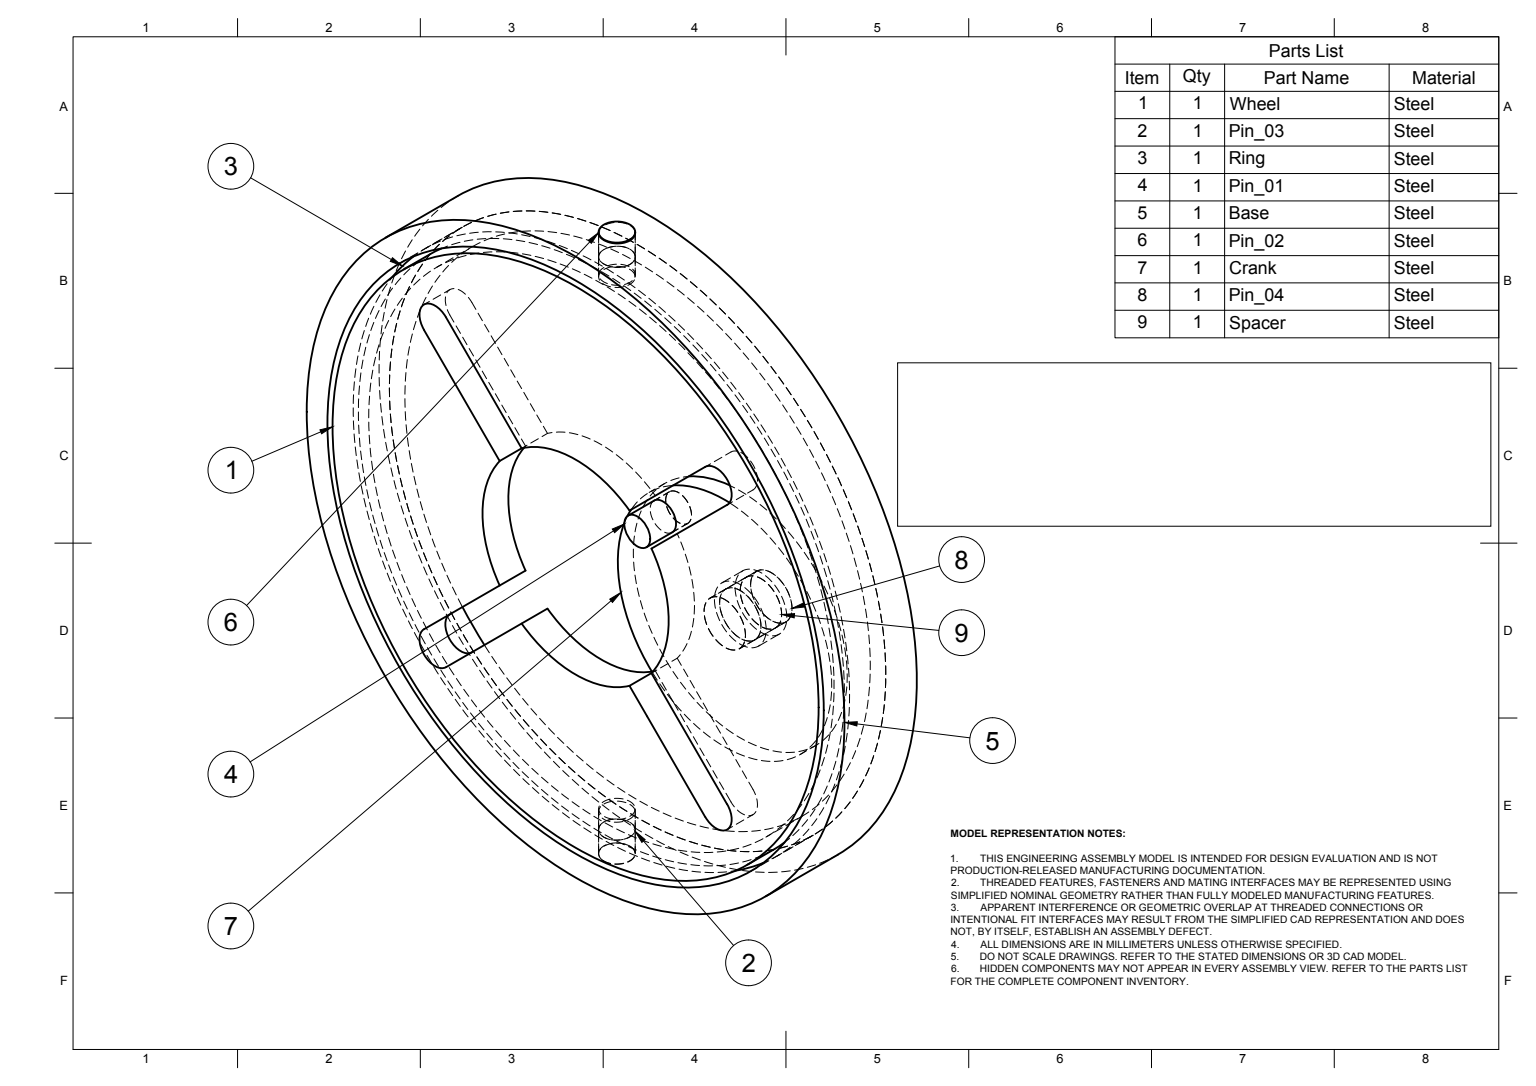
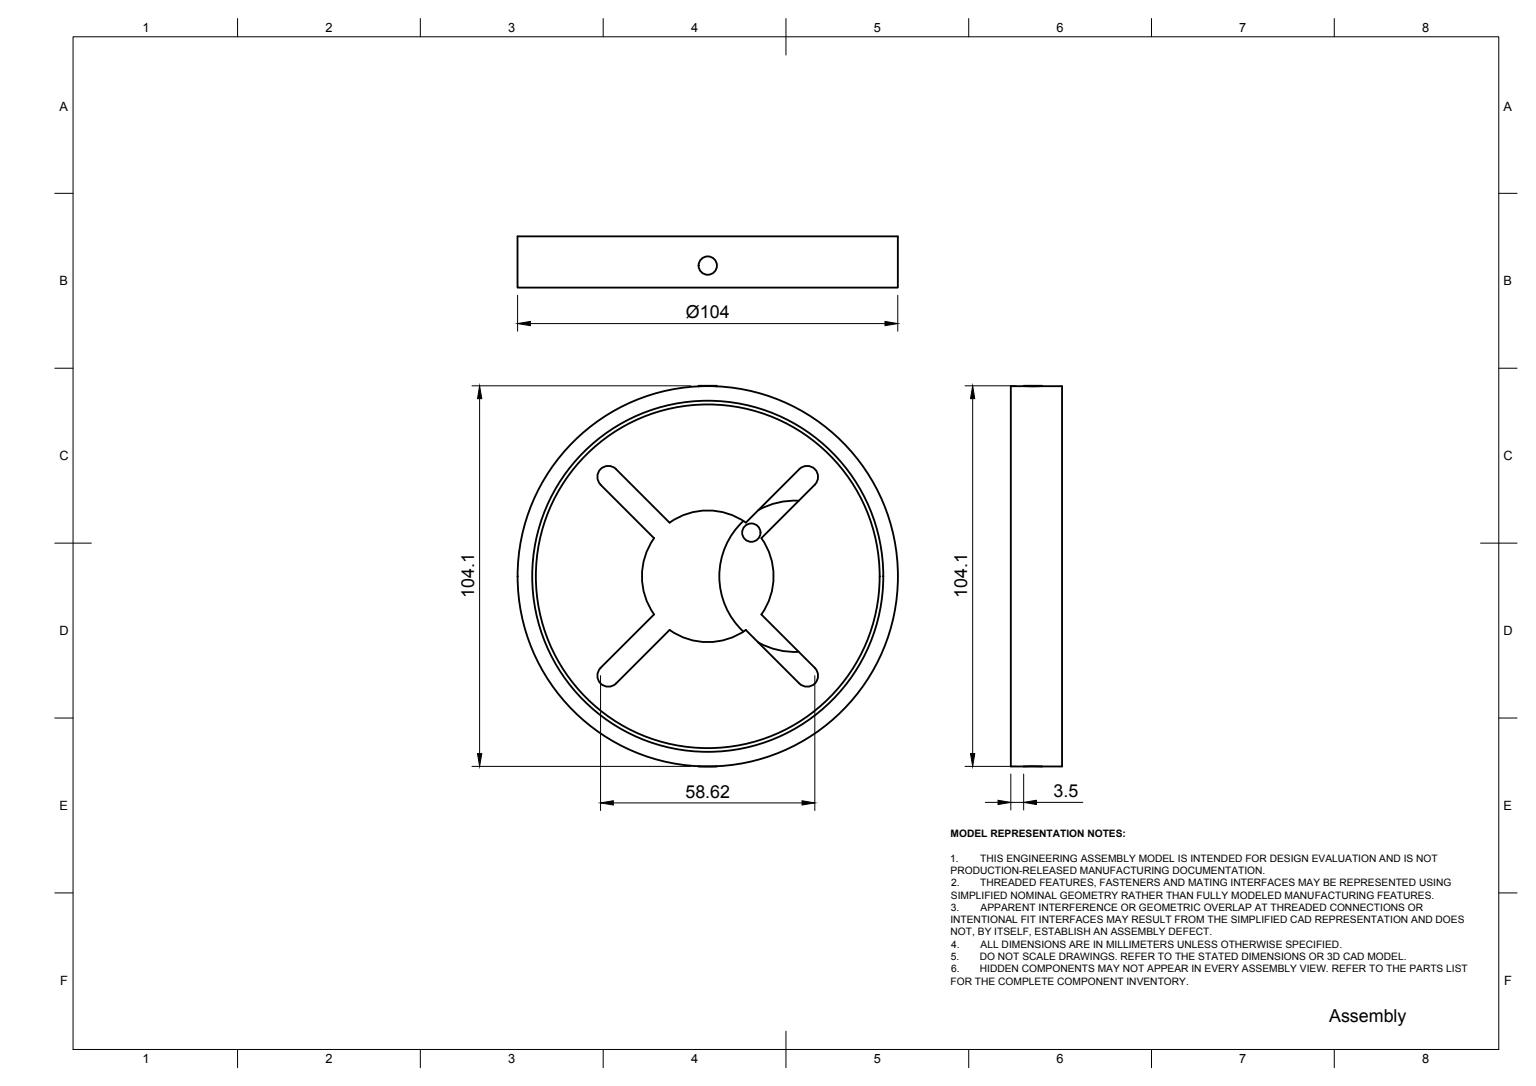
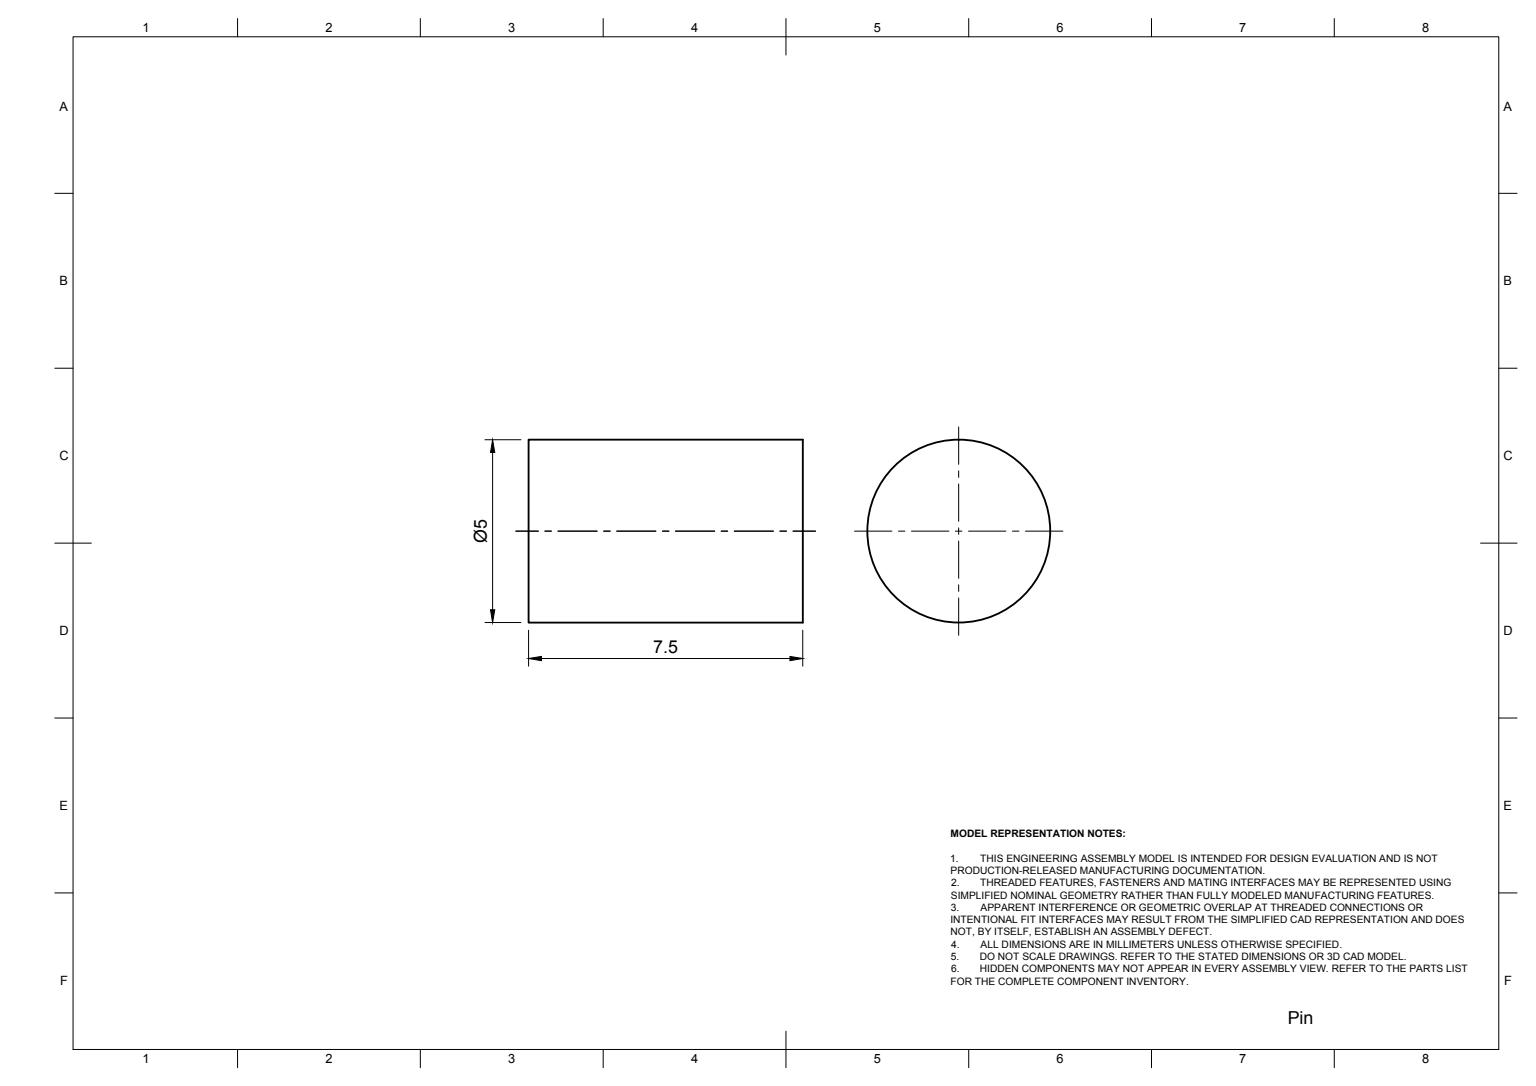
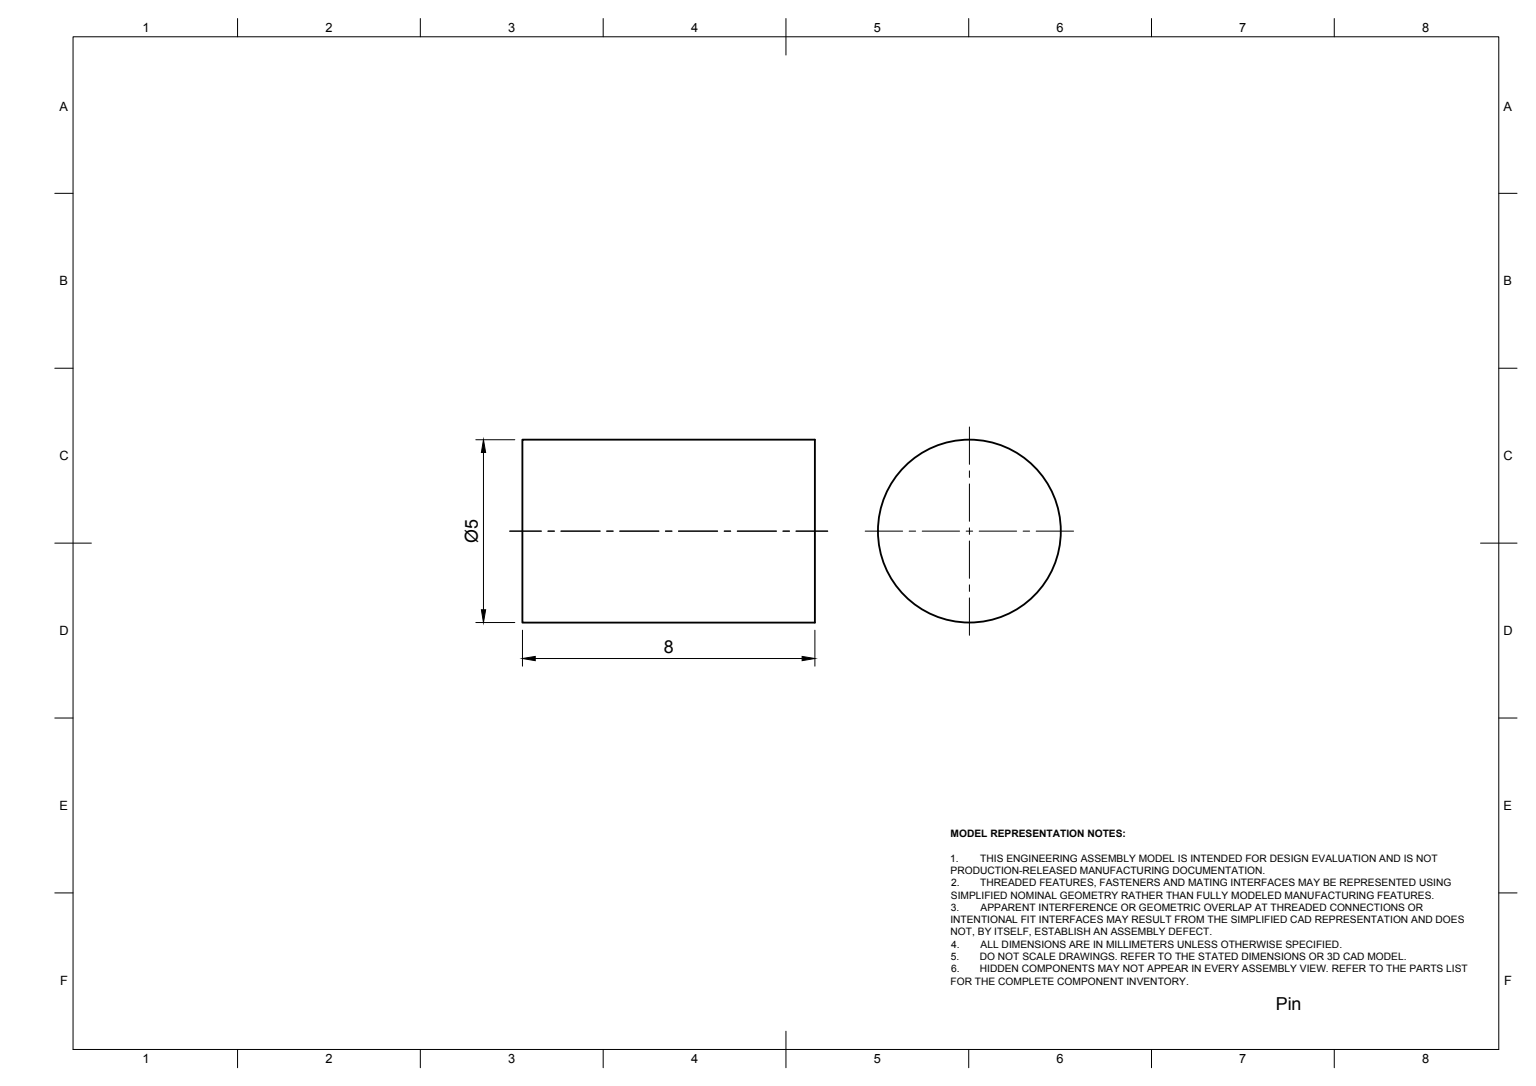
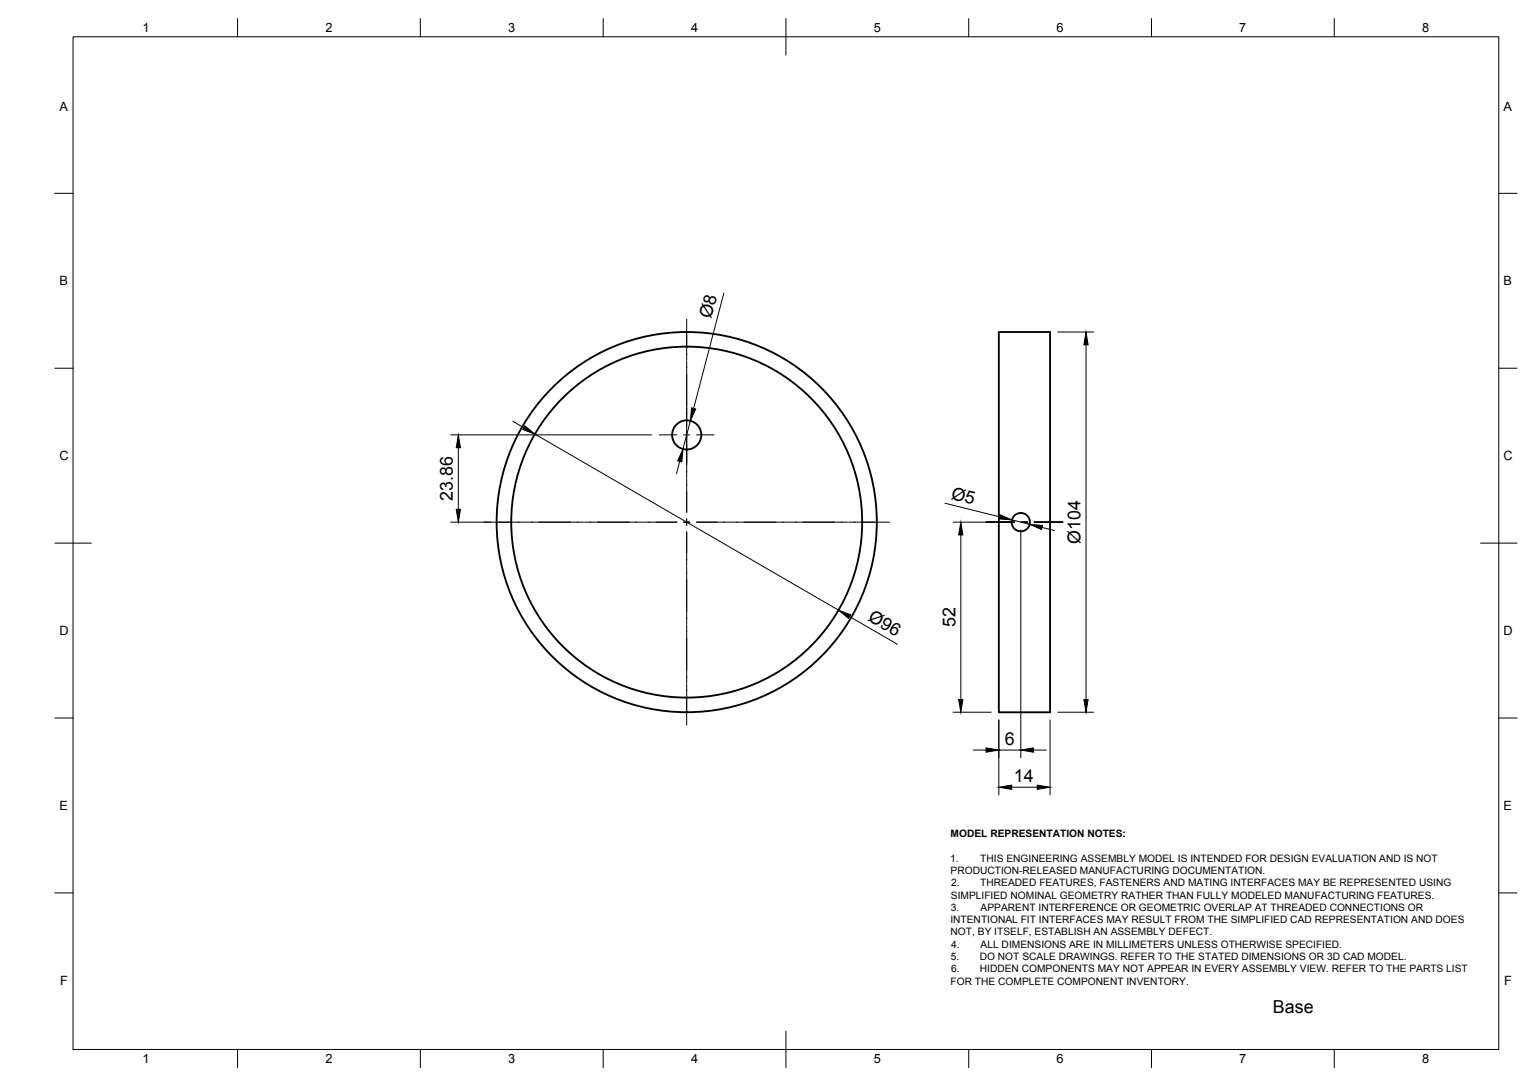
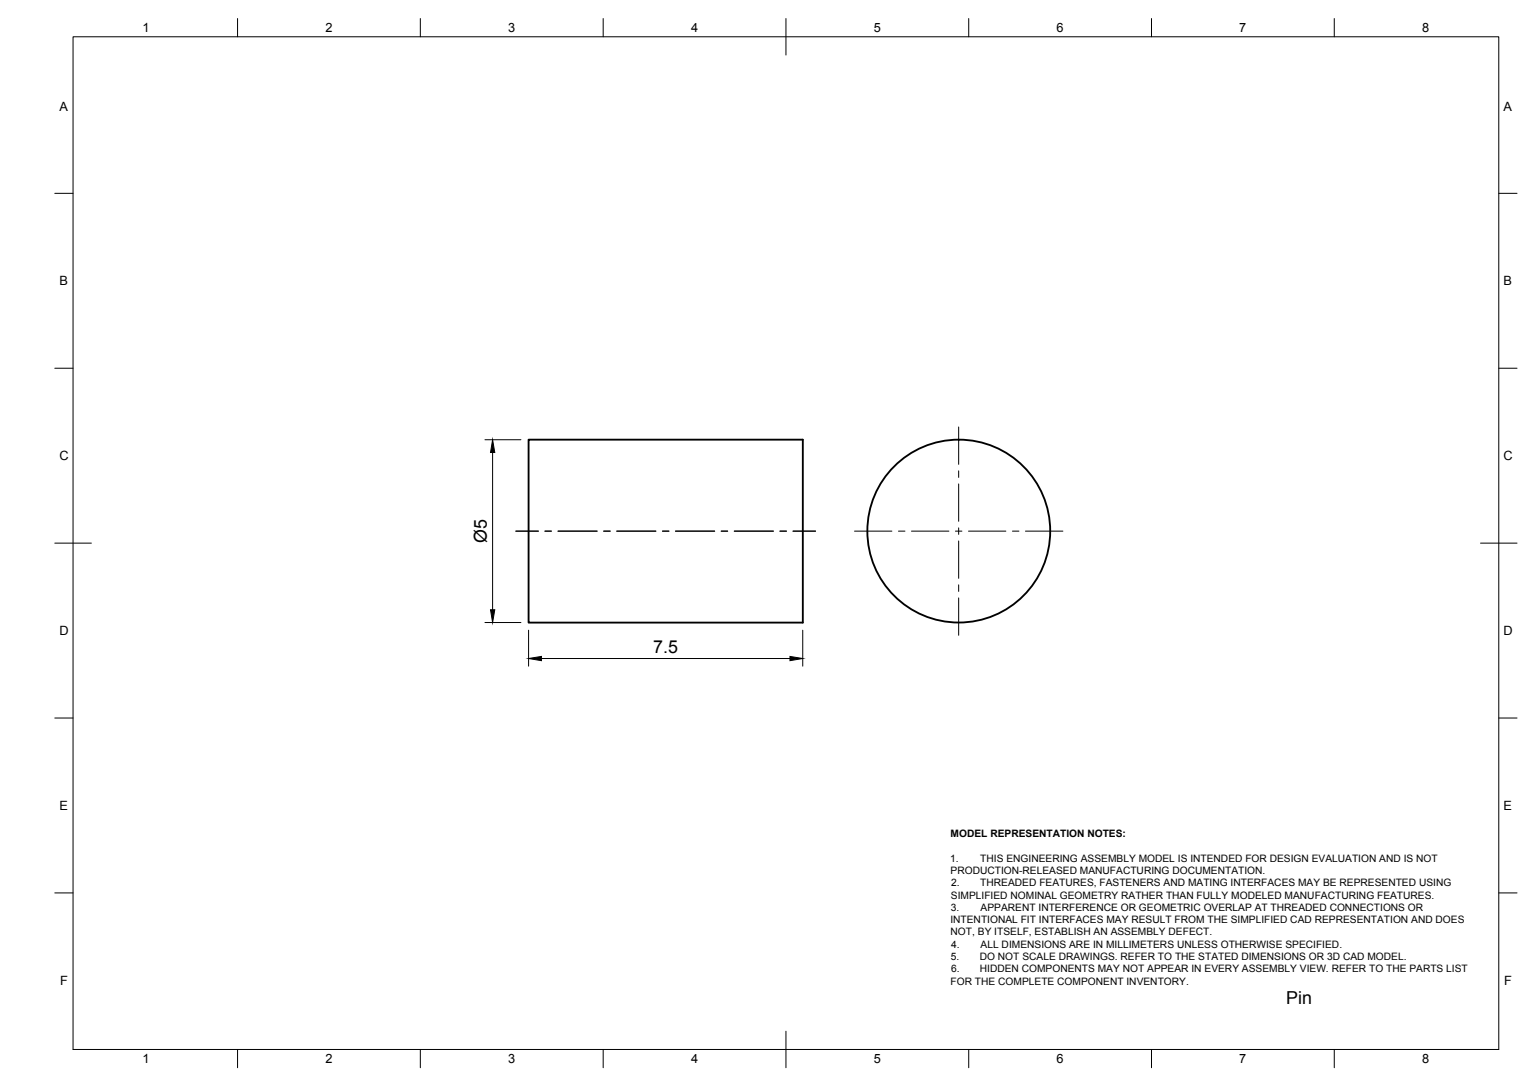
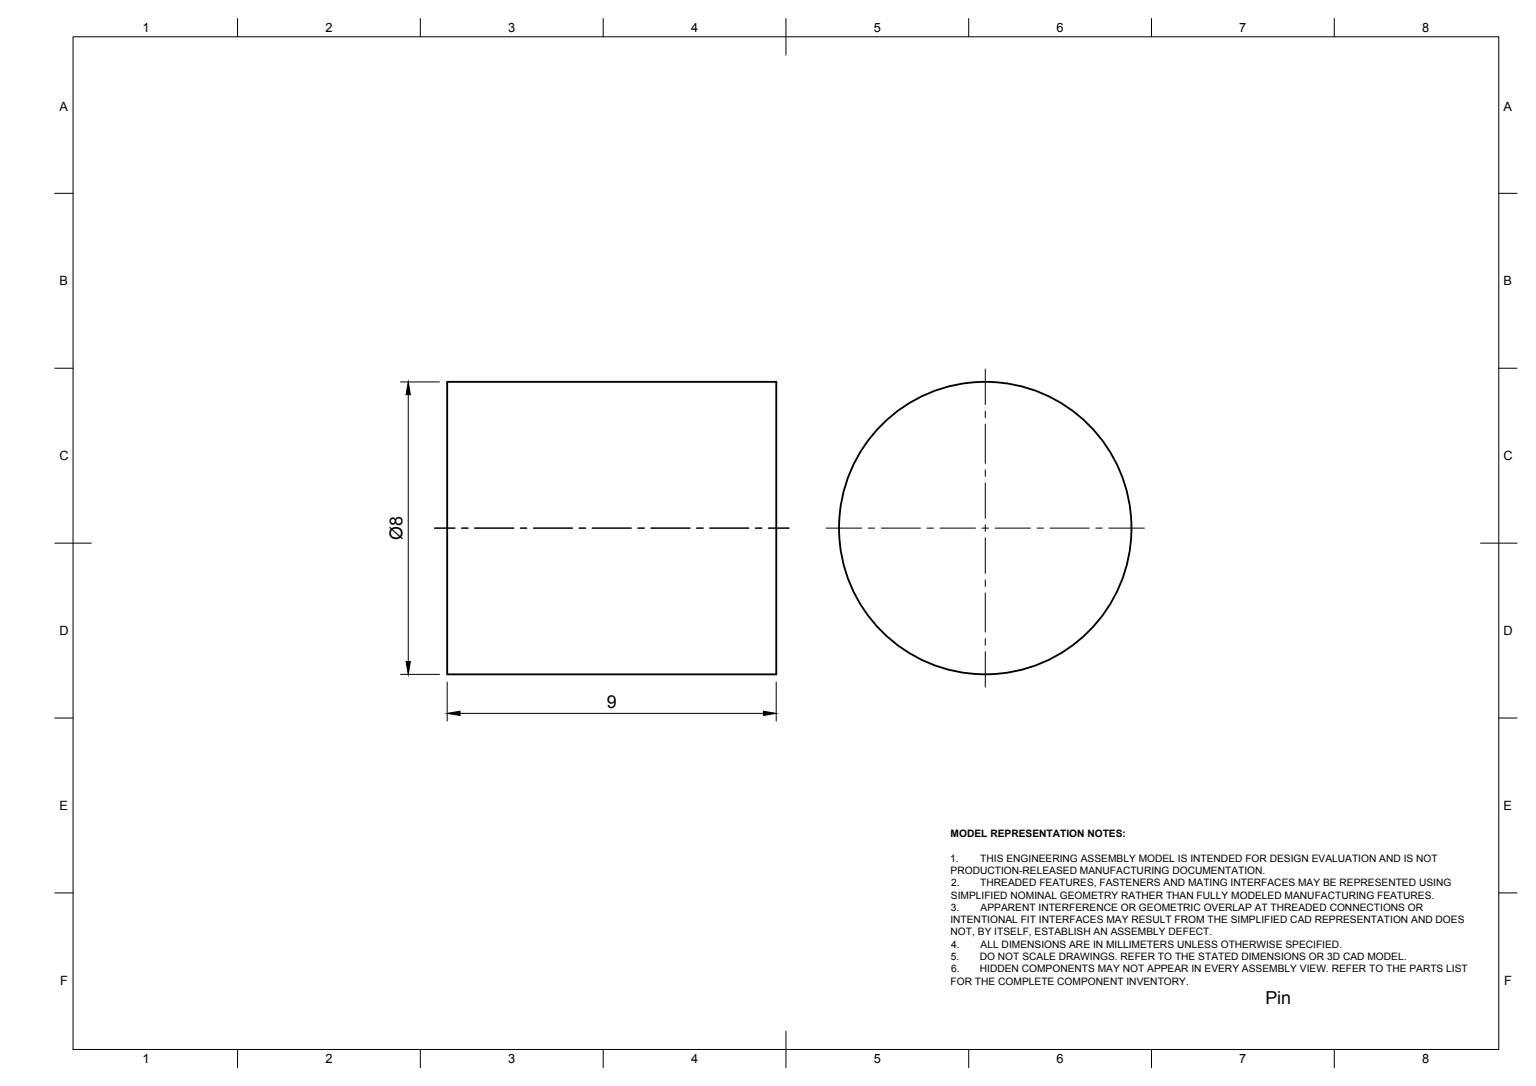
ISO-10303-21;
HEADER;
/* Generated by software containing ST-Developer
 * from STEP Tools, Inc. (www.steptools.com) 
 */

FILE_DESCRIPTION(
/* description */ (''),
/* implementation_level */ '2;1');

FILE_NAME(
/* name */ 'BR-053',
/* time_stamp */ '2026-10-04T12:17:52-07:00',
/* author */ (''),
/* organization */ (''),
/* preprocessor_version */ 'ST-DEVELOPER v20.2',
/* originating_system */ 'Autodesk Translation Framework v15.15.0.0',
/* authorisation */ '');

FILE_SCHEMA (('AUTOMOTIVE_DESIGN { 1 0 10303 214 3 1 1 }'));
ENDSEC;

DATA;
#10=MECHANICAL_DESIGN_GEOMETRIC_PRESENTATION_REPRESENTATION('',(#63,#64,
#65,#66,#67,#68,#69,#70),#1602);
#11=ITEM_DEFINED_TRANSFORMATION($,$,#872,#967);
#12=ITEM_DEFINED_TRANSFORMATION($,$,#911,#968);
#13=ITEM_DEFINED_TRANSFORMATION($,$,#917,#969);
#14=ITEM_DEFINED_TRANSFORMATION($,$,#928,#970);
#15=ITEM_DEFINED_TRANSFORMATION($,$,#934,#971);
#16=ITEM_DEFINED_TRANSFORMATION($,$,#940,#972);
#17=ITEM_DEFINED_TRANSFORMATION($,$,#952,#973);
#18=ITEM_DEFINED_TRANSFORMATION($,$,#958,#974);
#19=(
REPRESENTATION_RELATIONSHIP($,$,#1634,#1633)
REPRESENTATION_RELATIONSHIP_WITH_TRANSFORMATION(#11)
SHAPE_REPRESENTATION_RELATIONSHIP()
);
#20=(
REPRESENTATION_RELATIONSHIP($,$,#1635,#1633)
REPRESENTATION_RELATIONSHIP_WITH_TRANSFORMATION(#12)
SHAPE_REPRESENTATION_RELATIONSHIP()
);
#21=(
REPRESENTATION_RELATIONSHIP($,$,#1636,#1633)
REPRESENTATION_RELATIONSHIP_WITH_TRANSFORMATION(#13)
SHAPE_REPRESENTATION_RELATIONSHIP()
);
#22=(
REPRESENTATION_RELATIONSHIP($,$,#1637,#1633)
REPRESENTATION_RELATIONSHIP_WITH_TRANSFORMATION(#14)
SHAPE_REPRESENTATION_RELATIONSHIP()
);
#23=(
REPRESENTATION_RELATIONSHIP($,$,#1638,#1633)
REPRESENTATION_RELATIONSHIP_WITH_TRANSFORMATION(#15)
SHAPE_REPRESENTATION_RELATIONSHIP()
);
#24=(
REPRESENTATION_RELATIONSHIP($,$,#1639,#1633)
REPRESENTATION_RELATIONSHIP_WITH_TRANSFORMATION(#16)
SHAPE_REPRESENTATION_RELATIONSHIP()
);
#25=(
REPRESENTATION_RELATIONSHIP($,$,#1640,#1633)
REPRESENTATION_RELATIONSHIP_WITH_TRANSFORMATION(#17)
SHAPE_REPRESENTATION_RELATIONSHIP()
);
#26=(
REPRESENTATION_RELATIONSHIP($,$,#1641,#1633)
REPRESENTATION_RELATIONSHIP_WITH_TRANSFORMATION(#18)
SHAPE_REPRESENTATION_RELATIONSHIP()
);
#27=CONTEXT_DEPENDENT_SHAPE_REPRESENTATION(#19,#1625);
#28=CONTEXT_DEPENDENT_SHAPE_REPRESENTATION(#20,#1626);
#29=CONTEXT_DEPENDENT_SHAPE_REPRESENTATION(#21,#1627);
#30=CONTEXT_DEPENDENT_SHAPE_REPRESENTATION(#22,#1628);
#31=CONTEXT_DEPENDENT_SHAPE_REPRESENTATION(#23,#1629);
#32=CONTEXT_DEPENDENT_SHAPE_REPRESENTATION(#24,#1630);
#33=CONTEXT_DEPENDENT_SHAPE_REPRESENTATION(#25,#1631);
#34=CONTEXT_DEPENDENT_SHAPE_REPRESENTATION(#26,#1632);
#35=NEXT_ASSEMBLY_USAGE_OCCURRENCE('Wheel:1','Wheel:1','Wheel:1',#1643,
#1644,'Wheel:1');
#36=NEXT_ASSEMBLY_USAGE_OCCURRENCE('Pin_03:1','Pin_03:1','Pin_03:1',#1643,
#1645,'Pin_03:1');
#37=NEXT_ASSEMBLY_USAGE_OCCURRENCE('Ring:1','Ring:1','Ring:1',#1643,#1646,
'Ring:1');
#38=NEXT_ASSEMBLY_USAGE_OCCURRENCE('Pin_01:1','Pin_01:1','Pin_01:1',#1643,
#1647,'Pin_01:1');
#39=NEXT_ASSEMBLY_USAGE_OCCURRENCE('Pin_02:1','Pin_02:1','Pin_02:1',#1643,
#1648,'Pin_02:1');
#40=NEXT_ASSEMBLY_USAGE_OCCURRENCE('Crank:1','Crank:1','Crank:1',#1643,
#1649,'Crank:1');
#41=NEXT_ASSEMBLY_USAGE_OCCURRENCE('Pin_04:1','Pin_04:1','Pin_04:1',#1643,
#1650,'Pin_04:1');
#42=NEXT_ASSEMBLY_USAGE_OCCURRENCE('Spacer:1','Spacer:1','Spacer:1',#1643,
#1651,'Spacer:1');
#43=B_SPLINE_CURVE_WITH_KNOTS('',3,(#1356,#1357,#1358,#1359,#1360,#1361,
#1362,#1363,#1364,#1365,#1366,#1367,#1368,#1369,#1370,#1371,#1372,#1373,
#1374,#1375,#1376,#1377,#1378,#1379,#1380,#1381,#1382,#1383,#1384,#1385,
#1386,#1387,#1388,#1389),.UNSPECIFIED.,.T.,.F.,(4,2,2,2,2,2,2,2,2,2,2,2,
2,2,2,2,4),(0.,0.0941899649900925,0.188379929980185,0.282569871539204,0.376759813098223,
0.470949754657242,0.565139696216261,0.659329661206353,0.753519626196446,
0.847709591186538,0.941899556176631,1.03608949773565,1.13027943929467,1.22446938085369,
1.31865932241271,1.4128492874028,1.50703925239289),.UNSPECIFIED.);
#44=B_SPLINE_CURVE_WITH_KNOTS('',3,(#1392,#1393,#1394,#1395,#1396,#1397,
#1398,#1399,#1400,#1401,#1402,#1403,#1404,#1405,#1406,#1407,#1408,#1409,
#1410,#1411,#1412,#1413,#1414,#1415,#1416,#1417,#1418,#1419,#1420,#1421,
#1422,#1423,#1424,#1425),.UNSPECIFIED.,.T.,.F.,(4,2,2,2,2,2,2,2,2,2,2,2,
2,2,2,2,4),(-1.50707960704781,-1.41288711643541,-1.318694625823,-1.22450216555443,
-1.13030970528586,-1.03611724501729,-0.941924784748718,-0.847732294136312,
-0.753539803523906,-0.6593473129115,-0.565154822299094,-0.470962362030524,
-0.376769901761953,-0.282577441493383,-0.188384981224812,-0.094192490612406,
0.),.UNSPECIFIED.);
#45=B_SPLINE_CURVE_WITH_KNOTS('',3,(#1428,#1429,#1430,#1431,#1432,#1433,
#1434,#1435,#1436,#1437,#1438,#1439,#1440,#1441,#1442,#1443,#1444,#1445,
#1446,#1447,#1448,#1449,#1450,#1451,#1452,#1453,#1454,#1455,#1456,#1457,
#1458,#1459,#1460,#1461),.UNSPECIFIED.,.T.,.F.,(4,2,2,2,2,2,2,2,2,2,2,2,
2,2,2,2,4),(-1.50707960704781,-1.41288711643541,-1.318694625823,-1.22450216555443,
-1.13030970528586,-1.03611724501729,-0.941924784748719,-0.847732294136313,
-0.753539803523906,-0.6593473129115,-0.565154822299094,-0.470962362030524,
-0.376769901761953,-0.282577441493383,-0.188384981224812,-0.0941924906124062,
0.),.UNSPECIFIED.);
#46=B_SPLINE_CURVE_WITH_KNOTS('',3,(#1464,#1465,#1466,#1467,#1468,#1469,
#1470,#1471,#1472,#1473,#1474,#1475,#1476,#1477,#1478,#1479,#1480,#1481,
#1482,#1483,#1484,#1485,#1486,#1487,#1488,#1489,#1490,#1491,#1492,#1493,
#1494,#1495,#1496,#1497),.UNSPECIFIED.,.T.,.F.,(4,2,2,2,2,2,2,2,2,2,2,2,
2,2,2,2,4),(0.,0.0941899649900927,0.188379929980185,0.282569871539204,0.376759813098223,
0.470949754657242,0.565139696216261,0.659329661206353,0.753519626196446,
0.847709591186538,0.941899556176631,1.03608949773565,1.13027943929467,1.22446938085369,
1.31865932241271,1.4128492874028,1.50703925239289),.UNSPECIFIED.);
#47=SHAPE_REPRESENTATION_RELATIONSHIP('SRR','None',#1634,#55);
#48=SHAPE_REPRESENTATION_RELATIONSHIP('SRR','None',#1635,#56);
#49=SHAPE_REPRESENTATION_RELATIONSHIP('SRR','None',#1636,#57);
#50=SHAPE_REPRESENTATION_RELATIONSHIP('SRR','None',#1637,#58);
#51=SHAPE_REPRESENTATION_RELATIONSHIP('SRR','None',#1638,#59);
#52=SHAPE_REPRESENTATION_RELATIONSHIP('SRR','None',#1639,#60);
#53=SHAPE_REPRESENTATION_RELATIONSHIP('SRR','None',#1640,#61);
#54=SHAPE_REPRESENTATION_RELATIONSHIP('SRR','None',#1641,#62);
#55=ADVANCED_BREP_SHAPE_REPRESENTATION('',(#71),#1594);
#56=ADVANCED_BREP_SHAPE_REPRESENTATION('',(#72),#1595);
#57=ADVANCED_BREP_SHAPE_REPRESENTATION('',(#73),#1596);
#58=ADVANCED_BREP_SHAPE_REPRESENTATION('',(#74),#1597);
#59=ADVANCED_BREP_SHAPE_REPRESENTATION('',(#75),#1598);
#60=ADVANCED_BREP_SHAPE_REPRESENTATION('',(#76),#1599);
#61=ADVANCED_BREP_SHAPE_REPRESENTATION('',(#77),#1600);
#62=ADVANCED_BREP_SHAPE_REPRESENTATION('',(#78),#1601);
#63=STYLED_ITEM('',(#1683),#71);
#64=STYLED_ITEM('',(#1684),#72);
#65=STYLED_ITEM('',(#1684),#73);
#66=STYLED_ITEM('',(#1685),#74);
#67=STYLED_ITEM('',(#1684),#75);
#68=STYLED_ITEM('',(#1685),#76);
#69=STYLED_ITEM('',(#1684),#77);
#70=STYLED_ITEM('',(#1684),#78);
#71=MANIFOLD_SOLID_BREP('Body1',#774);
#72=MANIFOLD_SOLID_BREP('Body1',#775);
#73=MANIFOLD_SOLID_BREP('Body1',#776);
#74=MANIFOLD_SOLID_BREP('Body1',#777);
#75=MANIFOLD_SOLID_BREP('Body1',#778);
#76=MANIFOLD_SOLID_BREP('Body1',#779);
#77=MANIFOLD_SOLID_BREP('Body1',#780);
#78=MANIFOLD_SOLID_BREP('Body1',#781);
#79=FACE_BOUND('',#221,.T.);
#80=FACE_BOUND('',#223,.T.);
#81=FACE_BOUND('',#230,.T.);
#82=FACE_BOUND('',#231,.T.);
#83=FACE_BOUND('',#233,.T.);
#84=FACE_BOUND('',#234,.T.);
#85=FACE_BOUND('',#236,.T.);
#86=FACE_BOUND('',#238,.T.);
#87=FACE_BOUND('',#249,.T.);
#88=FACE_BOUND('',#250,.T.);
#89=FACE_BOUND('',#252,.T.);
#90=FACE_BOUND('',#253,.T.);
#91=FACE_BOUND('',#260,.T.);
#92=FACE_BOUND('',#262,.T.);
#93=CIRCLE('',#875,18.);
#94=CIRCLE('',#876,18.);
#95=CIRCLE('',#879,3.);
#96=CIRCLE('',#880,3.);
#97=CIRCLE('',#883,18.);
#98=CIRCLE('',#884,18.);
#99=CIRCLE('',#887,3.);
#100=CIRCLE('',#888,3.);
#101=CIRCLE('',#891,18.);
#102=CIRCLE('',#892,18.);
#103=CIRCLE('',#895,3.);
#104=CIRCLE('',#896,3.);
#105=CIRCLE('',#899,18.);
#106=CIRCLE('',#900,18.);
#107=CIRCLE('',#903,3.);
#108=CIRCLE('',#904,3.);
#109=CIRCLE('',#907,47.);
#110=CIRCLE('',#908,47.);
#111=CIRCLE('',#913,2.5);
#112=CIRCLE('',#915,2.5);
#113=CIRCLE('',#921,45.);
#114=CIRCLE('',#922,45.);
#115=CIRCLE('',#924,48.);
#116=CIRCLE('',#925,48.);
#117=CIRCLE('',#930,2.5);
#118=CIRCLE('',#932,2.5);
#119=CIRCLE('',#936,2.5);
#120=CIRCLE('',#938,2.5);
#121=CIRCLE('',#942,4.);
#122=CIRCLE('',#943,4.);
#123=CIRCLE('',#945,2.5);
#124=CIRCLE('',#946,2.5);
#125=CIRCLE('',#948,20.6801665756397);
#126=CIRCLE('',#949,20.6801665756397);
#127=CIRCLE('',#954,4.);
#128=CIRCLE('',#955,4.);
#129=CIRCLE('',#960,4.);
#130=CIRCLE('',#961,4.);
#131=CIRCLE('',#963,5.);
#132=CIRCLE('',#964,5.);
#133=CYLINDRICAL_SURFACE('',#874,18.);
#134=CYLINDRICAL_SURFACE('',#878,3.);
#135=CYLINDRICAL_SURFACE('',#882,18.);
#136=CYLINDRICAL_SURFACE('',#886,3.);
#137=CYLINDRICAL_SURFACE('',#890,18.);
#138=CYLINDRICAL_SURFACE('',#894,3.);
#139=CYLINDRICAL_SURFACE('',#898,18.);
#140=CYLINDRICAL_SURFACE('',#902,3.);
#141=CYLINDRICAL_SURFACE('',#906,47.);
#142=CYLINDRICAL_SURFACE('',#914,2.5);
#143=CYLINDRICAL_SURFACE('',#918,2.5);
#144=CYLINDRICAL_SURFACE('',#919,2.5);
#145=CYLINDRICAL_SURFACE('',#920,45.);
#146=CYLINDRICAL_SURFACE('',#923,48.);
#147=CYLINDRICAL_SURFACE('',#931,2.5);
#148=CYLINDRICAL_SURFACE('',#937,2.5);
#149=CYLINDRICAL_SURFACE('',#941,4.);
#150=CYLINDRICAL_SURFACE('',#944,2.5);
#151=CYLINDRICAL_SURFACE('',#947,20.6801665756397);
#152=CYLINDRICAL_SURFACE('',#953,4.);
#153=CYLINDRICAL_SURFACE('',#959,4.);
#154=CYLINDRICAL_SURFACE('',#962,5.);
#155=FACE_OUTER_BOUND('',#202,.T.);
#156=FACE_OUTER_BOUND('',#203,.T.);
#157=FACE_OUTER_BOUND('',#204,.T.);
#158=FACE_OUTER_BOUND('',#205,.T.);
#159=FACE_OUTER_BOUND('',#206,.T.);
#160=FACE_OUTER_BOUND('',#207,.T.);
#161=FACE_OUTER_BOUND('',#208,.T.);
#162=FACE_OUTER_BOUND('',#209,.T.);
#163=FACE_OUTER_BOUND('',#210,.T.);
#164=FACE_OUTER_BOUND('',#211,.T.);
#165=FACE_OUTER_BOUND('',#212,.T.);
#166=FACE_OUTER_BOUND('',#213,.T.);
#167=FACE_OUTER_BOUND('',#214,.T.);
#168=FACE_OUTER_BOUND('',#215,.T.);
#169=FACE_OUTER_BOUND('',#216,.T.);
#170=FACE_OUTER_BOUND('',#217,.T.);
#171=FACE_OUTER_BOUND('',#218,.T.);
#172=FACE_OUTER_BOUND('',#219,.T.);
#173=FACE_OUTER_BOUND('',#220,.T.);
#174=FACE_OUTER_BOUND('',#222,.T.);
#175=FACE_OUTER_BOUND('',#224,.T.);
#176=FACE_OUTER_BOUND('',#225,.T.);
#177=FACE_OUTER_BOUND('',#226,.T.);
#178=FACE_OUTER_BOUND('',#227,.T.);
#179=FACE_OUTER_BOUND('',#228,.T.);
#180=FACE_OUTER_BOUND('',#229,.T.);
#181=FACE_OUTER_BOUND('',#232,.T.);
#182=FACE_OUTER_BOUND('',#235,.T.);
#183=FACE_OUTER_BOUND('',#237,.T.);
#184=FACE_OUTER_BOUND('',#239,.T.);
#185=FACE_OUTER_BOUND('',#240,.T.);
#186=FACE_OUTER_BOUND('',#241,.T.);
#187=FACE_OUTER_BOUND('',#242,.T.);
#188=FACE_OUTER_BOUND('',#243,.T.);
#189=FACE_OUTER_BOUND('',#244,.T.);
#190=FACE_OUTER_BOUND('',#245,.T.);
#191=FACE_OUTER_BOUND('',#246,.T.);
#192=FACE_OUTER_BOUND('',#247,.T.);
#193=FACE_OUTER_BOUND('',#248,.T.);
#194=FACE_OUTER_BOUND('',#251,.T.);
#195=FACE_OUTER_BOUND('',#254,.T.);
#196=FACE_OUTER_BOUND('',#255,.T.);
#197=FACE_OUTER_BOUND('',#256,.T.);
#198=FACE_OUTER_BOUND('',#257,.T.);
#199=FACE_OUTER_BOUND('',#258,.T.);
#200=FACE_OUTER_BOUND('',#259,.T.);
#201=FACE_OUTER_BOUND('',#261,.T.);
#202=EDGE_LOOP('',(#516,#517,#518,#519));
#203=EDGE_LOOP('',(#520,#521,#522,#523));
#204=EDGE_LOOP('',(#524,#525,#526,#527));
#205=EDGE_LOOP('',(#528,#529,#530,#531));
#206=EDGE_LOOP('',(#532,#533,#534,#535));
#207=EDGE_LOOP('',(#536,#537,#538,#539));
#208=EDGE_LOOP('',(#540,#541,#542,#543));
#209=EDGE_LOOP('',(#544,#545,#546,#547));
#210=EDGE_LOOP('',(#548,#549,#550,#551));
#211=EDGE_LOOP('',(#552,#553,#554,#555));
#212=EDGE_LOOP('',(#556,#557,#558,#559));
#213=EDGE_LOOP('',(#560,#561,#562,#563));
#214=EDGE_LOOP('',(#564,#565,#566,#567));
#215=EDGE_LOOP('',(#568,#569,#570,#571));
#216=EDGE_LOOP('',(#572,#573,#574,#575));
#217=EDGE_LOOP('',(#576,#577,#578,#579));
#218=EDGE_LOOP('',(#580,#581,#582,#583));
#219=EDGE_LOOP('',(#584,#585,#586,#587));
#220=EDGE_LOOP('',(#588));
#221=EDGE_LOOP('',(#589,#590,#591,#592,#593,#594,#595,#596,#597,#598,#599,
#600,#601,#602,#603,#604,#605));
#222=EDGE_LOOP('',(#606));
#223=EDGE_LOOP('',(#607,#608,#609,#610,#611,#612,#613,#614,#615,#616,#617,
#618,#619,#620,#621,#622,#623));
#224=EDGE_LOOP('',(#624));
#225=EDGE_LOOP('',(#625,#626,#627,#628));
#226=EDGE_LOOP('',(#629));
#227=EDGE_LOOP('',(#630,#631,#632,#633));
#228=EDGE_LOOP('',(#634,#635,#636,#637));
#229=EDGE_LOOP('',(#638,#639,#640,#641));
#230=EDGE_LOOP('',(#642));
#231=EDGE_LOOP('',(#643));
#232=EDGE_LOOP('',(#644,#645,#646,#647));
#233=EDGE_LOOP('',(#648));
#234=EDGE_LOOP('',(#649));
#235=EDGE_LOOP('',(#650));
#236=EDGE_LOOP('',(#651));
#237=EDGE_LOOP('',(#652));
#238=EDGE_LOOP('',(#653));
#239=EDGE_LOOP('',(#654));
#240=EDGE_LOOP('',(#655,#656,#657,#658));
#241=EDGE_LOOP('',(#659));
#242=EDGE_LOOP('',(#660));
#243=EDGE_LOOP('',(#661,#662,#663,#664));
#244=EDGE_LOOP('',(#665));
#245=EDGE_LOOP('',(#666,#667,#668,#669));
#246=EDGE_LOOP('',(#670,#671,#672,#673));
#247=EDGE_LOOP('',(#674,#675,#676,#677));
#248=EDGE_LOOP('',(#678));
#249=EDGE_LOOP('',(#679));
#250=EDGE_LOOP('',(#680));
#251=EDGE_LOOP('',(#681));
#252=EDGE_LOOP('',(#682));
#253=EDGE_LOOP('',(#683));
#254=EDGE_LOOP('',(#684,#685,#686,#687));
#255=EDGE_LOOP('',(#688));
#256=EDGE_LOOP('',(#689));
#257=EDGE_LOOP('',(#690,#691,#692,#693));
#258=EDGE_LOOP('',(#694,#695,#696,#697));
#259=EDGE_LOOP('',(#698));
#260=EDGE_LOOP('',(#699));
#261=EDGE_LOOP('',(#700));
#262=EDGE_LOOP('',(#701));
#263=LINE('',#1237,#312);
#264=LINE('',#1239,#313);
#265=LINE('',#1241,#314);
#266=LINE('',#1242,#315);
#267=LINE('',#1248,#316);
#268=LINE('',#1251,#317);
#269=LINE('',#1254,#318);
#270=LINE('',#1256,#319);
#271=LINE('',#1257,#320);
#272=LINE('',#1263,#321);
#273=LINE('',#1266,#322);
#274=LINE('',#1268,#323);
#275=LINE('',#1269,#324);
#276=LINE('',#1275,#325);
#277=LINE('',#1278,#326);
#278=LINE('',#1280,#327);
#279=LINE('',#1281,#328);
#280=LINE('',#1287,#329);
#281=LINE('',#1290,#330);
#282=LINE('',#1292,#331);
#283=LINE('',#1293,#332);
#284=LINE('',#1299,#333);
#285=LINE('',#1302,#334);
#286=LINE('',#1304,#335);
#287=LINE('',#1305,#336);
#288=LINE('',#1311,#337);
#289=LINE('',#1314,#338);
#290=LINE('',#1316,#339);
#291=LINE('',#1317,#340);
#292=LINE('',#1323,#341);
#293=LINE('',#1325,#342);
#294=LINE('',#1326,#343);
#295=LINE('',#1332,#344);
#296=LINE('',#1334,#345);
#297=LINE('',#1335,#346);
#298=LINE('',#1340,#347);
#299=LINE('',#1351,#348);
#300=LINE('',#1391,#349);
#301=LINE('',#1463,#350);
#302=LINE('',#1502,#351);
#303=LINE('',#1508,#352);
#304=LINE('',#1518,#353);
#305=LINE('',#1528,#354);
#306=LINE('',#1535,#355);
#307=LINE('',#1541,#356);
#308=LINE('',#1547,#357);
#309=LINE('',#1556,#358);
#310=LINE('',#1565,#359);
#311=LINE('',#1571,#360);
#312=VECTOR('',#981,10.);
#313=VECTOR('',#982,10.);
#314=VECTOR('',#983,10.);
#315=VECTOR('',#984,10.);
#316=VECTOR('',#989,10.);
#317=VECTOR('',#992,10.);
#318=VECTOR('',#995,10.);
#319=VECTOR('',#996,10.);
#320=VECTOR('',#997,10.);
#321=VECTOR('',#1004,10.);
#322=VECTOR('',#1007,10.);
#323=VECTOR('',#1008,10.);
#324=VECTOR('',#1009,10.);
#325=VECTOR('',#1016,10.);
#326=VECTOR('',#1019,10.);
#327=VECTOR('',#1020,10.);
#328=VECTOR('',#1021,10.);
#329=VECTOR('',#1028,10.);
#330=VECTOR('',#1031,10.);
#331=VECTOR('',#1032,10.);
#332=VECTOR('',#1033,10.);
#333=VECTOR('',#1040,10.);
#334=VECTOR('',#1043,10.);
#335=VECTOR('',#1044,10.);
#336=VECTOR('',#1045,10.);
#337=VECTOR('',#1052,10.);
#338=VECTOR('',#1055,10.);
#339=VECTOR('',#1056,10.);
#340=VECTOR('',#1057,10.);
#341=VECTOR('',#1066,10.);
#342=VECTOR('',#1067,10.);
#343=VECTOR('',#1068,10.);
#344=VECTOR('',#1075,10.);
#345=VECTOR('',#1078,10.);
#346=VECTOR('',#1079,10.);
#347=VECTOR('',#1084,47.);
#348=VECTOR('',#1101,2.5);
#349=VECTOR('',#1108,2.5);
#350=VECTOR('',#1111,2.5);
#351=VECTOR('',#1116,45.);
#352=VECTOR('',#1123,48.);
#353=VECTOR('',#1138,2.5);
#354=VECTOR('',#1153,2.5);
#355=VECTOR('',#1162,4.);
#356=VECTOR('',#1169,2.5);
#357=VECTOR('',#1176,20.6801665756397);
#358=VECTOR('',#1189,4.);
#359=VECTOR('',#1202,4.);
#360=VECTOR('',#1209,5.);
#361=VERTEX_POINT('',#1235);
#362=VERTEX_POINT('',#1236);
#363=VERTEX_POINT('',#1238);
#364=VERTEX_POINT('',#1240);
#365=VERTEX_POINT('',#1244);
#366=VERTEX_POINT('',#1245);
#367=VERTEX_POINT('',#1247);
#368=VERTEX_POINT('',#1249);
#369=VERTEX_POINT('',#1253);
#370=VERTEX_POINT('',#1255);
#371=VERTEX_POINT('',#1259);
#372=VERTEX_POINT('',#1261);
#373=VERTEX_POINT('',#1265);
#374=VERTEX_POINT('',#1267);
#375=VERTEX_POINT('',#1271);
#376=VERTEX_POINT('',#1273);
#377=VERTEX_POINT('',#1277);
#378=VERTEX_POINT('',#1279);
#379=VERTEX_POINT('',#1283);
#380=VERTEX_POINT('',#1285);
#381=VERTEX_POINT('',#1289);
#382=VERTEX_POINT('',#1291);
#383=VERTEX_POINT('',#1295);
#384=VERTEX_POINT('',#1297);
#385=VERTEX_POINT('',#1301);
#386=VERTEX_POINT('',#1303);
#387=VERTEX_POINT('',#1307);
#388=VERTEX_POINT('',#1309);
#389=VERTEX_POINT('',#1313);
#390=VERTEX_POINT('',#1315);
#391=VERTEX_POINT('',#1322);
#392=VERTEX_POINT('',#1324);
#393=VERTEX_POINT('',#1328);
#394=VERTEX_POINT('',#1330);
#395=VERTEX_POINT('',#1337);
#396=VERTEX_POINT('',#1339);
#397=VERTEX_POINT('',#1346);
#398=VERTEX_POINT('',#1349);
#399=VERTEX_POINT('',#1355);
#400=VERTEX_POINT('',#1390);
#401=VERTEX_POINT('',#1427);
#402=VERTEX_POINT('',#1462);
#403=VERTEX_POINT('',#1499);
#404=VERTEX_POINT('',#1501);
#405=VERTEX_POINT('',#1505);
#406=VERTEX_POINT('',#1507);
#407=VERTEX_POINT('',#1514);
#408=VERTEX_POINT('',#1517);
#409=VERTEX_POINT('',#1523);
#410=VERTEX_POINT('',#1526);
#411=VERTEX_POINT('',#1532);
#412=VERTEX_POINT('',#1534);
#413=VERTEX_POINT('',#1538);
#414=VERTEX_POINT('',#1540);
#415=VERTEX_POINT('',#1544);
#416=VERTEX_POINT('',#1546);
#417=VERTEX_POINT('',#1553);
#418=VERTEX_POINT('',#1555);
#419=VERTEX_POINT('',#1562);
#420=VERTEX_POINT('',#1564);
#421=VERTEX_POINT('',#1568);
#422=VERTEX_POINT('',#1570);
#423=EDGE_CURVE('',#361,#362,#263,.T.);
#424=EDGE_CURVE('',#363,#362,#264,.T.);
#425=EDGE_CURVE('',#364,#363,#265,.T.);
#426=EDGE_CURVE('',#361,#364,#266,.T.);
#427=EDGE_CURVE('',#365,#366,#93,.T.);
#428=EDGE_CURVE('',#365,#367,#267,.T.);
#429=EDGE_CURVE('',#368,#367,#94,.T.);
#430=EDGE_CURVE('',#366,#368,#268,.T.);
#431=EDGE_CURVE('',#366,#369,#269,.T.);
#432=EDGE_CURVE('',#370,#368,#270,.T.);
#433=EDGE_CURVE('',#369,#370,#271,.T.);
#434=EDGE_CURVE('',#369,#371,#95,.T.);
#435=EDGE_CURVE('',#372,#370,#96,.T.);
#436=EDGE_CURVE('',#371,#372,#272,.T.);
#437=EDGE_CURVE('',#371,#373,#273,.T.);
#438=EDGE_CURVE('',#374,#372,#274,.T.);
#439=EDGE_CURVE('',#374,#373,#275,.T.);
#440=EDGE_CURVE('',#373,#375,#97,.T.);
#441=EDGE_CURVE('',#374,#376,#98,.T.);
#442=EDGE_CURVE('',#375,#376,#276,.T.);
#443=EDGE_CURVE('',#375,#377,#277,.T.);
#444=EDGE_CURVE('',#378,#376,#278,.T.);
#445=EDGE_CURVE('',#377,#378,#279,.T.);
#446=EDGE_CURVE('',#377,#379,#99,.T.);
#447=EDGE_CURVE('',#380,#378,#100,.T.);
#448=EDGE_CURVE('',#379,#380,#280,.T.);
#449=EDGE_CURVE('',#379,#381,#281,.T.);
#450=EDGE_CURVE('',#382,#380,#282,.T.);
#451=EDGE_CURVE('',#381,#382,#283,.T.);
#452=EDGE_CURVE('',#381,#383,#101,.T.);
#453=EDGE_CURVE('',#384,#382,#102,.T.);
#454=EDGE_CURVE('',#383,#384,#284,.T.);
#455=EDGE_CURVE('',#383,#385,#285,.T.);
#456=EDGE_CURVE('',#386,#384,#286,.T.);
#457=EDGE_CURVE('',#385,#386,#287,.T.);
#458=EDGE_CURVE('',#385,#387,#103,.T.);
#459=EDGE_CURVE('',#388,#386,#104,.T.);
#460=EDGE_CURVE('',#387,#388,#288,.T.);
#461=EDGE_CURVE('',#387,#389,#289,.T.);
#462=EDGE_CURVE('',#390,#388,#290,.T.);
#463=EDGE_CURVE('',#389,#390,#291,.T.);
#464=EDGE_CURVE('',#389,#362,#105,.T.);
#465=EDGE_CURVE('',#363,#390,#106,.T.);
#466=EDGE_CURVE('',#361,#391,#292,.T.);
#467=EDGE_CURVE('',#392,#364,#293,.T.);
#468=EDGE_CURVE('',#391,#392,#294,.T.);
#469=EDGE_CURVE('',#391,#393,#107,.T.);
#470=EDGE_CURVE('',#394,#392,#108,.T.);
#471=EDGE_CURVE('',#393,#394,#295,.T.);
#472=EDGE_CURVE('',#393,#365,#296,.T.);
#473=EDGE_CURVE('',#367,#394,#297,.T.);
#474=EDGE_CURVE('',#395,#395,#109,.T.);
#475=EDGE_CURVE('',#395,#396,#298,.T.);
#476=EDGE_CURVE('',#396,#396,#110,.T.);
#477=EDGE_CURVE('',#397,#397,#111,.T.);
#478=EDGE_CURVE('',#398,#398,#112,.T.);
#479=EDGE_CURVE('',#398,#397,#299,.T.);
#480=EDGE_CURVE('',#399,#399,#43,.T.);
#481=EDGE_CURVE('',#399,#400,#300,.T.);
#482=EDGE_CURVE('',#400,#400,#44,.T.);
#483=EDGE_CURVE('',#401,#401,#45,.T.);
#484=EDGE_CURVE('',#401,#402,#301,.T.);
#485=EDGE_CURVE('',#402,#402,#46,.T.);
#486=EDGE_CURVE('',#403,#403,#113,.T.);
#487=EDGE_CURVE('',#403,#404,#302,.T.);
#488=EDGE_CURVE('',#404,#404,#114,.T.);
#489=EDGE_CURVE('',#405,#405,#115,.T.);
#490=EDGE_CURVE('',#405,#406,#303,.T.);
#491=EDGE_CURVE('',#406,#406,#116,.T.);
#492=EDGE_CURVE('',#407,#407,#117,.T.);
#493=EDGE_CURVE('',#407,#408,#304,.T.);
#494=EDGE_CURVE('',#408,#408,#118,.T.);
#495=EDGE_CURVE('',#409,#409,#119,.T.);
#496=EDGE_CURVE('',#410,#410,#120,.T.);
#497=EDGE_CURVE('',#410,#409,#305,.T.);
#498=EDGE_CURVE('',#411,#411,#121,.T.);
#499=EDGE_CURVE('',#411,#412,#306,.T.);
#500=EDGE_CURVE('',#412,#412,#122,.T.);
#501=EDGE_CURVE('',#413,#413,#123,.T.);
#502=EDGE_CURVE('',#413,#414,#307,.T.);
#503=EDGE_CURVE('',#414,#414,#124,.T.);
#504=EDGE_CURVE('',#415,#415,#125,.T.);
#505=EDGE_CURVE('',#415,#416,#308,.T.);
#506=EDGE_CURVE('',#416,#416,#126,.T.);
#507=EDGE_CURVE('',#417,#417,#127,.T.);
#508=EDGE_CURVE('',#417,#418,#309,.T.);
#509=EDGE_CURVE('',#418,#418,#128,.T.);
#510=EDGE_CURVE('',#419,#419,#129,.T.);
#511=EDGE_CURVE('',#419,#420,#310,.T.);
#512=EDGE_CURVE('',#420,#420,#130,.T.);
#513=EDGE_CURVE('',#421,#421,#131,.T.);
#514=EDGE_CURVE('',#421,#422,#311,.T.);
#515=EDGE_CURVE('',#422,#422,#132,.T.);
#516=ORIENTED_EDGE('',*,*,#423,.T.);
#517=ORIENTED_EDGE('',*,*,#424,.F.);
#518=ORIENTED_EDGE('',*,*,#425,.F.);
#519=ORIENTED_EDGE('',*,*,#426,.F.);
#520=ORIENTED_EDGE('',*,*,#427,.F.);
#521=ORIENTED_EDGE('',*,*,#428,.T.);
#522=ORIENTED_EDGE('',*,*,#429,.F.);
#523=ORIENTED_EDGE('',*,*,#430,.F.);
#524=ORIENTED_EDGE('',*,*,#431,.F.);
#525=ORIENTED_EDGE('',*,*,#430,.T.);
#526=ORIENTED_EDGE('',*,*,#432,.F.);
#527=ORIENTED_EDGE('',*,*,#433,.F.);
#528=ORIENTED_EDGE('',*,*,#434,.F.);
#529=ORIENTED_EDGE('',*,*,#433,.T.);
#530=ORIENTED_EDGE('',*,*,#435,.F.);
#531=ORIENTED_EDGE('',*,*,#436,.F.);
#532=ORIENTED_EDGE('',*,*,#437,.F.);
#533=ORIENTED_EDGE('',*,*,#436,.T.);
#534=ORIENTED_EDGE('',*,*,#438,.F.);
#535=ORIENTED_EDGE('',*,*,#439,.T.);
#536=ORIENTED_EDGE('',*,*,#440,.F.);
#537=ORIENTED_EDGE('',*,*,#439,.F.);
#538=ORIENTED_EDGE('',*,*,#441,.T.);
#539=ORIENTED_EDGE('',*,*,#442,.F.);
#540=ORIENTED_EDGE('',*,*,#443,.F.);
#541=ORIENTED_EDGE('',*,*,#442,.T.);
#542=ORIENTED_EDGE('',*,*,#444,.F.);
#543=ORIENTED_EDGE('',*,*,#445,.F.);
#544=ORIENTED_EDGE('',*,*,#446,.F.);
#545=ORIENTED_EDGE('',*,*,#445,.T.);
#546=ORIENTED_EDGE('',*,*,#447,.F.);
#547=ORIENTED_EDGE('',*,*,#448,.F.);
#548=ORIENTED_EDGE('',*,*,#449,.F.);
#549=ORIENTED_EDGE('',*,*,#448,.T.);
#550=ORIENTED_EDGE('',*,*,#450,.F.);
#551=ORIENTED_EDGE('',*,*,#451,.F.);
#552=ORIENTED_EDGE('',*,*,#452,.F.);
#553=ORIENTED_EDGE('',*,*,#451,.T.);
#554=ORIENTED_EDGE('',*,*,#453,.F.);
#555=ORIENTED_EDGE('',*,*,#454,.F.);
#556=ORIENTED_EDGE('',*,*,#455,.F.);
#557=ORIENTED_EDGE('',*,*,#454,.T.);
#558=ORIENTED_EDGE('',*,*,#456,.F.);
#559=ORIENTED_EDGE('',*,*,#457,.F.);
#560=ORIENTED_EDGE('',*,*,#458,.F.);
#561=ORIENTED_EDGE('',*,*,#457,.T.);
#562=ORIENTED_EDGE('',*,*,#459,.F.);
#563=ORIENTED_EDGE('',*,*,#460,.F.);
#564=ORIENTED_EDGE('',*,*,#461,.F.);
#565=ORIENTED_EDGE('',*,*,#460,.T.);
#566=ORIENTED_EDGE('',*,*,#462,.F.);
#567=ORIENTED_EDGE('',*,*,#463,.F.);
#568=ORIENTED_EDGE('',*,*,#464,.F.);
#569=ORIENTED_EDGE('',*,*,#463,.T.);
#570=ORIENTED_EDGE('',*,*,#465,.F.);
#571=ORIENTED_EDGE('',*,*,#424,.T.);
#572=ORIENTED_EDGE('',*,*,#466,.F.);
#573=ORIENTED_EDGE('',*,*,#426,.T.);
#574=ORIENTED_EDGE('',*,*,#467,.F.);
#575=ORIENTED_EDGE('',*,*,#468,.F.);
#576=ORIENTED_EDGE('',*,*,#469,.F.);
#577=ORIENTED_EDGE('',*,*,#468,.T.);
#578=ORIENTED_EDGE('',*,*,#470,.F.);
#579=ORIENTED_EDGE('',*,*,#471,.F.);
#580=ORIENTED_EDGE('',*,*,#472,.F.);
#581=ORIENTED_EDGE('',*,*,#471,.T.);
#582=ORIENTED_EDGE('',*,*,#473,.F.);
#583=ORIENTED_EDGE('',*,*,#428,.F.);
#584=ORIENTED_EDGE('',*,*,#474,.F.);
#585=ORIENTED_EDGE('',*,*,#475,.T.);
#586=ORIENTED_EDGE('',*,*,#476,.F.);
#587=ORIENTED_EDGE('',*,*,#475,.F.);
#588=ORIENTED_EDGE('',*,*,#476,.T.);
#589=ORIENTED_EDGE('',*,*,#472,.T.);
#590=ORIENTED_EDGE('',*,*,#427,.T.);
#591=ORIENTED_EDGE('',*,*,#431,.T.);
#592=ORIENTED_EDGE('',*,*,#434,.T.);
#593=ORIENTED_EDGE('',*,*,#437,.T.);
#594=ORIENTED_EDGE('',*,*,#440,.T.);
#595=ORIENTED_EDGE('',*,*,#443,.T.);
#596=ORIENTED_EDGE('',*,*,#446,.T.);
#597=ORIENTED_EDGE('',*,*,#449,.T.);
#598=ORIENTED_EDGE('',*,*,#452,.T.);
#599=ORIENTED_EDGE('',*,*,#455,.T.);
#600=ORIENTED_EDGE('',*,*,#458,.T.);
#601=ORIENTED_EDGE('',*,*,#461,.T.);
#602=ORIENTED_EDGE('',*,*,#464,.T.);
#603=ORIENTED_EDGE('',*,*,#423,.F.);
#604=ORIENTED_EDGE('',*,*,#466,.T.);
#605=ORIENTED_EDGE('',*,*,#469,.T.);
#606=ORIENTED_EDGE('',*,*,#474,.T.);
#607=ORIENTED_EDGE('',*,*,#473,.T.);
#608=ORIENTED_EDGE('',*,*,#470,.T.);
#609=ORIENTED_EDGE('',*,*,#467,.T.);
#610=ORIENTED_EDGE('',*,*,#425,.T.);
#611=ORIENTED_EDGE('',*,*,#465,.T.);
#612=ORIENTED_EDGE('',*,*,#462,.T.);
#613=ORIENTED_EDGE('',*,*,#459,.T.);
#614=ORIENTED_EDGE('',*,*,#456,.T.);
#615=ORIENTED_EDGE('',*,*,#453,.T.);
#616=ORIENTED_EDGE('',*,*,#450,.T.);
#617=ORIENTED_EDGE('',*,*,#447,.T.);
#618=ORIENTED_EDGE('',*,*,#444,.T.);
#619=ORIENTED_EDGE('',*,*,#441,.F.);
#620=ORIENTED_EDGE('',*,*,#438,.T.);
#621=ORIENTED_EDGE('',*,*,#435,.T.);
#622=ORIENTED_EDGE('',*,*,#432,.T.);
#623=ORIENTED_EDGE('',*,*,#429,.T.);
#624=ORIENTED_EDGE('',*,*,#477,.T.);
#625=ORIENTED_EDGE('',*,*,#478,.F.);
#626=ORIENTED_EDGE('',*,*,#479,.T.);
#627=ORIENTED_EDGE('',*,*,#477,.F.);
#628=ORIENTED_EDGE('',*,*,#479,.F.);
#629=ORIENTED_EDGE('',*,*,#478,.T.);
#630=ORIENTED_EDGE('',*,*,#480,.F.);
#631=ORIENTED_EDGE('',*,*,#481,.T.);
#632=ORIENTED_EDGE('',*,*,#482,.F.);
#633=ORIENTED_EDGE('',*,*,#481,.F.);
#634=ORIENTED_EDGE('',*,*,#483,.F.);
#635=ORIENTED_EDGE('',*,*,#484,.T.);
#636=ORIENTED_EDGE('',*,*,#485,.F.);
#637=ORIENTED_EDGE('',*,*,#484,.F.);
#638=ORIENTED_EDGE('',*,*,#486,.T.);
#639=ORIENTED_EDGE('',*,*,#487,.T.);
#640=ORIENTED_EDGE('',*,*,#488,.F.);
#641=ORIENTED_EDGE('',*,*,#487,.F.);
#642=ORIENTED_EDGE('',*,*,#482,.T.);
#643=ORIENTED_EDGE('',*,*,#483,.T.);
#644=ORIENTED_EDGE('',*,*,#489,.F.);
#645=ORIENTED_EDGE('',*,*,#490,.T.);
#646=ORIENTED_EDGE('',*,*,#491,.T.);
#647=ORIENTED_EDGE('',*,*,#490,.F.);
#648=ORIENTED_EDGE('',*,*,#480,.T.);
#649=ORIENTED_EDGE('',*,*,#485,.T.);
#650=ORIENTED_EDGE('',*,*,#489,.T.);
#651=ORIENTED_EDGE('',*,*,#488,.T.);
#652=ORIENTED_EDGE('',*,*,#491,.F.);
#653=ORIENTED_EDGE('',*,*,#486,.F.);
#654=ORIENTED_EDGE('',*,*,#492,.T.);
#655=ORIENTED_EDGE('',*,*,#492,.F.);
#656=ORIENTED_EDGE('',*,*,#493,.T.);
#657=ORIENTED_EDGE('',*,*,#494,.T.);
#658=ORIENTED_EDGE('',*,*,#493,.F.);
#659=ORIENTED_EDGE('',*,*,#494,.F.);
#660=ORIENTED_EDGE('',*,*,#495,.T.);
#661=ORIENTED_EDGE('',*,*,#496,.F.);
#662=ORIENTED_EDGE('',*,*,#497,.T.);
#663=ORIENTED_EDGE('',*,*,#495,.F.);
#664=ORIENTED_EDGE('',*,*,#497,.F.);
#665=ORIENTED_EDGE('',*,*,#496,.T.);
#666=ORIENTED_EDGE('',*,*,#498,.F.);
#667=ORIENTED_EDGE('',*,*,#499,.T.);
#668=ORIENTED_EDGE('',*,*,#500,.F.);
#669=ORIENTED_EDGE('',*,*,#499,.F.);
#670=ORIENTED_EDGE('',*,*,#501,.F.);
#671=ORIENTED_EDGE('',*,*,#502,.T.);
#672=ORIENTED_EDGE('',*,*,#503,.F.);
#673=ORIENTED_EDGE('',*,*,#502,.F.);
#674=ORIENTED_EDGE('',*,*,#504,.F.);
#675=ORIENTED_EDGE('',*,*,#505,.T.);
#676=ORIENTED_EDGE('',*,*,#506,.T.);
#677=ORIENTED_EDGE('',*,*,#505,.F.);
#678=ORIENTED_EDGE('',*,*,#504,.T.);
#679=ORIENTED_EDGE('',*,*,#500,.T.);
#680=ORIENTED_EDGE('',*,*,#501,.T.);
#681=ORIENTED_EDGE('',*,*,#506,.F.);
#682=ORIENTED_EDGE('',*,*,#498,.T.);
#683=ORIENTED_EDGE('',*,*,#503,.T.);
#684=ORIENTED_EDGE('',*,*,#507,.F.);
#685=ORIENTED_EDGE('',*,*,#508,.T.);
#686=ORIENTED_EDGE('',*,*,#509,.T.);
#687=ORIENTED_EDGE('',*,*,#508,.F.);
#688=ORIENTED_EDGE('',*,*,#507,.T.);
#689=ORIENTED_EDGE('',*,*,#509,.F.);
#690=ORIENTED_EDGE('',*,*,#510,.T.);
#691=ORIENTED_EDGE('',*,*,#511,.T.);
#692=ORIENTED_EDGE('',*,*,#512,.F.);
#693=ORIENTED_EDGE('',*,*,#511,.F.);
#694=ORIENTED_EDGE('',*,*,#513,.F.);
#695=ORIENTED_EDGE('',*,*,#514,.T.);
#696=ORIENTED_EDGE('',*,*,#515,.T.);
#697=ORIENTED_EDGE('',*,*,#514,.F.);
#698=ORIENTED_EDGE('',*,*,#513,.T.);
#699=ORIENTED_EDGE('',*,*,#512,.T.);
#700=ORIENTED_EDGE('',*,*,#515,.F.);
#701=ORIENTED_EDGE('',*,*,#510,.F.);
#702=PLANE('',#873);
#703=PLANE('',#877);
#704=PLANE('',#881);
#705=PLANE('',#885);
#706=PLANE('',#889);
#707=PLANE('',#893);
#708=PLANE('',#897);
#709=PLANE('',#901);
#710=PLANE('',#905);
#711=PLANE('',#909);
#712=PLANE('',#910);
#713=PLANE('',#912);
#714=PLANE('',#916);
#715=PLANE('',#926);
#716=PLANE('',#927);
#717=PLANE('',#929);
#718=PLANE('',#933);
#719=PLANE('',#935);
#720=PLANE('',#939);
#721=PLANE('',#950);
#722=PLANE('',#951);
#723=PLANE('',#956);
#724=PLANE('',#957);
#725=PLANE('',#965);
#726=PLANE('',#966);
#727=ADVANCED_FACE('',(#155),#702,.T.);
#728=ADVANCED_FACE('',(#156),#133,.F.);
#729=ADVANCED_FACE('',(#157),#703,.T.);
#730=ADVANCED_FACE('',(#158),#134,.F.);
#731=ADVANCED_FACE('',(#159),#704,.T.);
#732=ADVANCED_FACE('',(#160),#135,.F.);
#733=ADVANCED_FACE('',(#161),#705,.T.);
#734=ADVANCED_FACE('',(#162),#136,.F.);
#735=ADVANCED_FACE('',(#163),#706,.T.);
#736=ADVANCED_FACE('',(#164),#137,.F.);
#737=ADVANCED_FACE('',(#165),#707,.T.);
#738=ADVANCED_FACE('',(#166),#138,.F.);
#739=ADVANCED_FACE('',(#167),#708,.T.);
#740=ADVANCED_FACE('',(#168),#139,.F.);
#741=ADVANCED_FACE('',(#169),#709,.T.);
#742=ADVANCED_FACE('',(#170),#140,.F.);
#743=ADVANCED_FACE('',(#171),#710,.T.);
#744=ADVANCED_FACE('',(#172),#141,.T.);
#745=ADVANCED_FACE('',(#173,#79),#711,.T.);
#746=ADVANCED_FACE('',(#174,#80),#712,.F.);
#747=ADVANCED_FACE('',(#175),#713,.F.);
#748=ADVANCED_FACE('',(#176),#142,.T.);
#749=ADVANCED_FACE('',(#177),#714,.T.);
#750=ADVANCED_FACE('',(#178),#143,.F.);
#751=ADVANCED_FACE('',(#179),#144,.F.);
#752=ADVANCED_FACE('',(#180,#81,#82),#145,.F.);
#753=ADVANCED_FACE('',(#181,#83,#84),#146,.T.);
#754=ADVANCED_FACE('',(#182,#85),#715,.T.);
#755=ADVANCED_FACE('',(#183,#86),#716,.F.);
#756=ADVANCED_FACE('',(#184),#717,.F.);
#757=ADVANCED_FACE('',(#185),#147,.T.);
#758=ADVANCED_FACE('',(#186),#718,.T.);
#759=ADVANCED_FACE('',(#187),#719,.F.);
#760=ADVANCED_FACE('',(#188),#148,.T.);
#761=ADVANCED_FACE('',(#189),#720,.T.);
#762=ADVANCED_FACE('',(#190),#149,.F.);
#763=ADVANCED_FACE('',(#191),#150,.F.);
#764=ADVANCED_FACE('',(#192),#151,.T.);
#765=ADVANCED_FACE('',(#193,#87,#88),#721,.T.);
#766=ADVANCED_FACE('',(#194,#89,#90),#722,.F.);
#767=ADVANCED_FACE('',(#195),#152,.T.);
#768=ADVANCED_FACE('',(#196),#723,.T.);
#769=ADVANCED_FACE('',(#197),#724,.F.);
#770=ADVANCED_FACE('',(#198),#153,.F.);
#771=ADVANCED_FACE('',(#199),#154,.T.);
#772=ADVANCED_FACE('',(#200,#91),#725,.T.);
#773=ADVANCED_FACE('',(#201,#92),#726,.F.);
#774=CLOSED_SHELL('',(#727,#728,#729,#730,#731,#732,#733,#734,#735,#736,
#737,#738,#739,#740,#741,#742,#743,#744,#745,#746));
#775=CLOSED_SHELL('',(#747,#748,#749));
#776=CLOSED_SHELL('',(#750,#751,#752,#753,#754,#755));
#777=CLOSED_SHELL('',(#756,#757,#758));
#778=CLOSED_SHELL('',(#759,#760,#761));
#779=CLOSED_SHELL('',(#762,#763,#764,#765,#766));
#780=CLOSED_SHELL('',(#767,#768,#769));
#781=CLOSED_SHELL('',(#770,#771,#772,#773));
#782=DERIVED_UNIT_ELEMENT(#798,1.);
#783=DERIVED_UNIT_ELEMENT(#1604,-3.);
#784=DERIVED_UNIT_ELEMENT(#798,1.);
#785=DERIVED_UNIT_ELEMENT(#1604,-3.);
#786=DERIVED_UNIT_ELEMENT(#798,1.);
#787=DERIVED_UNIT_ELEMENT(#1604,-3.);
#788=DERIVED_UNIT_ELEMENT(#798,1.);
#789=DERIVED_UNIT_ELEMENT(#1604,-3.);
#790=DERIVED_UNIT_ELEMENT(#798,1.);
#791=DERIVED_UNIT_ELEMENT(#1604,-3.);
#792=DERIVED_UNIT_ELEMENT(#798,1.);
#793=DERIVED_UNIT_ELEMENT(#1604,-3.);
#794=DERIVED_UNIT_ELEMENT(#798,1.);
#795=DERIVED_UNIT_ELEMENT(#1604,-3.);
#796=DERIVED_UNIT_ELEMENT(#798,1.);
#797=DERIVED_UNIT_ELEMENT(#1604,-3.);
#798=(
MASS_UNIT()
NAMED_UNIT(*)
SI_UNIT(.KILO.,.GRAM.)
);
#799=DERIVED_UNIT((#782,#783));
#800=DERIVED_UNIT((#784,#785));
#801=DERIVED_UNIT((#786,#787));
#802=DERIVED_UNIT((#788,#789));
#803=DERIVED_UNIT((#790,#791));
#804=DERIVED_UNIT((#792,#793));
#805=DERIVED_UNIT((#794,#795));
#806=DERIVED_UNIT((#796,#797));
#807=MEASURE_REPRESENTATION_ITEM('density measure',
POSITIVE_RATIO_MEASURE(7850.),#799);
#808=MEASURE_REPRESENTATION_ITEM('density measure',
POSITIVE_RATIO_MEASURE(7850.),#800);
#809=MEASURE_REPRESENTATION_ITEM('density measure',
POSITIVE_RATIO_MEASURE(7850.),#801);
#810=MEASURE_REPRESENTATION_ITEM('density measure',
POSITIVE_RATIO_MEASURE(7850.),#802);
#811=MEASURE_REPRESENTATION_ITEM('density measure',
POSITIVE_RATIO_MEASURE(7850.),#803);
#812=MEASURE_REPRESENTATION_ITEM('density measure',
POSITIVE_RATIO_MEASURE(7850.),#804);
#813=MEASURE_REPRESENTATION_ITEM('density measure',
POSITIVE_RATIO_MEASURE(7850.),#805);
#814=MEASURE_REPRESENTATION_ITEM('density measure',
POSITIVE_RATIO_MEASURE(7850.),#806);
#815=PROPERTY_DEFINITION_REPRESENTATION(#855,#831);
#816=PROPERTY_DEFINITION_REPRESENTATION(#856,#832);
#817=PROPERTY_DEFINITION_REPRESENTATION(#857,#833);
#818=PROPERTY_DEFINITION_REPRESENTATION(#858,#834);
#819=PROPERTY_DEFINITION_REPRESENTATION(#859,#835);
#820=PROPERTY_DEFINITION_REPRESENTATION(#860,#836);
#821=PROPERTY_DEFINITION_REPRESENTATION(#861,#837);
#822=PROPERTY_DEFINITION_REPRESENTATION(#862,#838);
#823=PROPERTY_DEFINITION_REPRESENTATION(#863,#839);
#824=PROPERTY_DEFINITION_REPRESENTATION(#864,#840);
#825=PROPERTY_DEFINITION_REPRESENTATION(#865,#841);
#826=PROPERTY_DEFINITION_REPRESENTATION(#866,#842);
#827=PROPERTY_DEFINITION_REPRESENTATION(#867,#843);
#828=PROPERTY_DEFINITION_REPRESENTATION(#868,#844);
#829=PROPERTY_DEFINITION_REPRESENTATION(#869,#845);
#830=PROPERTY_DEFINITION_REPRESENTATION(#870,#846);
#831=REPRESENTATION('material name',(#847),#1594);
#832=REPRESENTATION('density',(#807),#1594);
#833=REPRESENTATION('material name',(#848),#1595);
#834=REPRESENTATION('density',(#808),#1595);
#835=REPRESENTATION('material name',(#849),#1596);
#836=REPRESENTATION('density',(#809),#1596);
#837=REPRESENTATION('material name',(#850),#1597);
#838=REPRESENTATION('density',(#810),#1597);
#839=REPRESENTATION('material name',(#851),#1598);
#840=REPRESENTATION('density',(#811),#1598);
#841=REPRESENTATION('material name',(#852),#1599);
#842=REPRESENTATION('density',(#812),#1599);
#843=REPRESENTATION('material name',(#853),#1600);
#844=REPRESENTATION('density',(#813),#1600);
#845=REPRESENTATION('material name',(#854),#1601);
#846=REPRESENTATION('density',(#814),#1601);
#847=DESCRIPTIVE_REPRESENTATION_ITEM('Steel','Steel');
#848=DESCRIPTIVE_REPRESENTATION_ITEM('Steel','Steel');
#849=DESCRIPTIVE_REPRESENTATION_ITEM('Steel','Steel');
#850=DESCRIPTIVE_REPRESENTATION_ITEM('Steel','Steel');
#851=DESCRIPTIVE_REPRESENTATION_ITEM('Steel','Steel');
#852=DESCRIPTIVE_REPRESENTATION_ITEM('Steel','Steel');
#853=DESCRIPTIVE_REPRESENTATION_ITEM('Steel','Steel');
#854=DESCRIPTIVE_REPRESENTATION_ITEM('Steel','Steel');
#855=PROPERTY_DEFINITION('material property','material name',#1644);
#856=PROPERTY_DEFINITION('material property','density of part',#1644);
#857=PROPERTY_DEFINITION('material property','material name',#1645);
#858=PROPERTY_DEFINITION('material property','density of part',#1645);
#859=PROPERTY_DEFINITION('material property','material name',#1646);
#860=PROPERTY_DEFINITION('material property','density of part',#1646);
#861=PROPERTY_DEFINITION('material property','material name',#1647);
#862=PROPERTY_DEFINITION('material property','density of part',#1647);
#863=PROPERTY_DEFINITION('material property','material name',#1648);
#864=PROPERTY_DEFINITION('material property','density of part',#1648);
#865=PROPERTY_DEFINITION('material property','material name',#1649);
#866=PROPERTY_DEFINITION('material property','density of part',#1649);
#867=PROPERTY_DEFINITION('material property','material name',#1650);
#868=PROPERTY_DEFINITION('material property','density of part',#1650);
#869=PROPERTY_DEFINITION('material property','material name',#1651);
#870=PROPERTY_DEFINITION('material property','density of part',#1651);
#871=AXIS2_PLACEMENT_3D('',#1232,#975,#976);
#872=AXIS2_PLACEMENT_3D('',#1233,#977,#978);
#873=AXIS2_PLACEMENT_3D('',#1234,#979,#980);
#874=AXIS2_PLACEMENT_3D('',#1243,#985,#986);
#875=AXIS2_PLACEMENT_3D('',#1246,#987,#988);
#876=AXIS2_PLACEMENT_3D('',#1250,#990,#991);
#877=AXIS2_PLACEMENT_3D('',#1252,#993,#994);
#878=AXIS2_PLACEMENT_3D('',#1258,#998,#999);
#879=AXIS2_PLACEMENT_3D('',#1260,#1000,#1001);
#880=AXIS2_PLACEMENT_3D('',#1262,#1002,#1003);
#881=AXIS2_PLACEMENT_3D('',#1264,#1005,#1006);
#882=AXIS2_PLACEMENT_3D('',#1270,#1010,#1011);
#883=AXIS2_PLACEMENT_3D('',#1272,#1012,#1013);
#884=AXIS2_PLACEMENT_3D('',#1274,#1014,#1015);
#885=AXIS2_PLACEMENT_3D('',#1276,#1017,#1018);
#886=AXIS2_PLACEMENT_3D('',#1282,#1022,#1023);
#887=AXIS2_PLACEMENT_3D('',#1284,#1024,#1025);
#888=AXIS2_PLACEMENT_3D('',#1286,#1026,#1027);
#889=AXIS2_PLACEMENT_3D('',#1288,#1029,#1030);
#890=AXIS2_PLACEMENT_3D('',#1294,#1034,#1035);
#891=AXIS2_PLACEMENT_3D('',#1296,#1036,#1037);
#892=AXIS2_PLACEMENT_3D('',#1298,#1038,#1039);
#893=AXIS2_PLACEMENT_3D('',#1300,#1041,#1042);
#894=AXIS2_PLACEMENT_3D('',#1306,#1046,#1047);
#895=AXIS2_PLACEMENT_3D('',#1308,#1048,#1049);
#896=AXIS2_PLACEMENT_3D('',#1310,#1050,#1051);
#897=AXIS2_PLACEMENT_3D('',#1312,#1053,#1054);
#898=AXIS2_PLACEMENT_3D('',#1318,#1058,#1059);
#899=AXIS2_PLACEMENT_3D('',#1319,#1060,#1061);
#900=AXIS2_PLACEMENT_3D('',#1320,#1062,#1063);
#901=AXIS2_PLACEMENT_3D('',#1321,#1064,#1065);
#902=AXIS2_PLACEMENT_3D('',#1327,#1069,#1070);
#903=AXIS2_PLACEMENT_3D('',#1329,#1071,#1072);
#904=AXIS2_PLACEMENT_3D('',#1331,#1073,#1074);
#905=AXIS2_PLACEMENT_3D('',#1333,#1076,#1077);
#906=AXIS2_PLACEMENT_3D('',#1336,#1080,#1081);
#907=AXIS2_PLACEMENT_3D('',#1338,#1082,#1083);
#908=AXIS2_PLACEMENT_3D('',#1341,#1085,#1086);
#909=AXIS2_PLACEMENT_3D('',#1342,#1087,#1088);
#910=AXIS2_PLACEMENT_3D('',#1343,#1089,#1090);
#911=AXIS2_PLACEMENT_3D('',#1344,#1091,#1092);
#912=AXIS2_PLACEMENT_3D('',#1345,#1093,#1094);
#913=AXIS2_PLACEMENT_3D('',#1347,#1095,#1096);
#914=AXIS2_PLACEMENT_3D('',#1348,#1097,#1098);
#915=AXIS2_PLACEMENT_3D('',#1350,#1099,#1100);
#916=AXIS2_PLACEMENT_3D('',#1352,#1102,#1103);
#917=AXIS2_PLACEMENT_3D('',#1353,#1104,#1105);
#918=AXIS2_PLACEMENT_3D('',#1354,#1106,#1107);
#919=AXIS2_PLACEMENT_3D('',#1426,#1109,#1110);
#920=AXIS2_PLACEMENT_3D('',#1498,#1112,#1113);
#921=AXIS2_PLACEMENT_3D('',#1500,#1114,#1115);
#922=AXIS2_PLACEMENT_3D('',#1503,#1117,#1118);
#923=AXIS2_PLACEMENT_3D('',#1504,#1119,#1120);
#924=AXIS2_PLACEMENT_3D('',#1506,#1121,#1122);
#925=AXIS2_PLACEMENT_3D('',#1509,#1124,#1125);
#926=AXIS2_PLACEMENT_3D('',#1510,#1126,#1127);
#927=AXIS2_PLACEMENT_3D('',#1511,#1128,#1129);
#928=AXIS2_PLACEMENT_3D('',#1512,#1130,#1131);
#929=AXIS2_PLACEMENT_3D('',#1513,#1132,#1133);
#930=AXIS2_PLACEMENT_3D('',#1515,#1134,#1135);
#931=AXIS2_PLACEMENT_3D('',#1516,#1136,#1137);
#932=AXIS2_PLACEMENT_3D('',#1519,#1139,#1140);
#933=AXIS2_PLACEMENT_3D('',#1520,#1141,#1142);
#934=AXIS2_PLACEMENT_3D('',#1521,#1143,#1144);
#935=AXIS2_PLACEMENT_3D('',#1522,#1145,#1146);
#936=AXIS2_PLACEMENT_3D('',#1524,#1147,#1148);
#937=AXIS2_PLACEMENT_3D('',#1525,#1149,#1150);
#938=AXIS2_PLACEMENT_3D('',#1527,#1151,#1152);
#939=AXIS2_PLACEMENT_3D('',#1529,#1154,#1155);
#940=AXIS2_PLACEMENT_3D('',#1530,#1156,#1157);
#941=AXIS2_PLACEMENT_3D('',#1531,#1158,#1159);
#942=AXIS2_PLACEMENT_3D('',#1533,#1160,#1161);
#943=AXIS2_PLACEMENT_3D('',#1536,#1163,#1164);
#944=AXIS2_PLACEMENT_3D('',#1537,#1165,#1166);
#945=AXIS2_PLACEMENT_3D('',#1539,#1167,#1168);
#946=AXIS2_PLACEMENT_3D('',#1542,#1170,#1171);
#947=AXIS2_PLACEMENT_3D('',#1543,#1172,#1173);
#948=AXIS2_PLACEMENT_3D('',#1545,#1174,#1175);
#949=AXIS2_PLACEMENT_3D('',#1548,#1177,#1178);
#950=AXIS2_PLACEMENT_3D('',#1549,#1179,#1180);
#951=AXIS2_PLACEMENT_3D('',#1550,#1181,#1182);
#952=AXIS2_PLACEMENT_3D('',#1551,#1183,#1184);
#953=AXIS2_PLACEMENT_3D('',#1552,#1185,#1186);
#954=AXIS2_PLACEMENT_3D('',#1554,#1187,#1188);
#955=AXIS2_PLACEMENT_3D('',#1557,#1190,#1191);
#956=AXIS2_PLACEMENT_3D('',#1558,#1192,#1193);
#957=AXIS2_PLACEMENT_3D('',#1559,#1194,#1195);
#958=AXIS2_PLACEMENT_3D('',#1560,#1196,#1197);
#959=AXIS2_PLACEMENT_3D('',#1561,#1198,#1199);
#960=AXIS2_PLACEMENT_3D('',#1563,#1200,#1201);
#961=AXIS2_PLACEMENT_3D('',#1566,#1203,#1204);
#962=AXIS2_PLACEMENT_3D('',#1567,#1205,#1206);
#963=AXIS2_PLACEMENT_3D('',#1569,#1207,#1208);
#964=AXIS2_PLACEMENT_3D('',#1572,#1210,#1211);
#965=AXIS2_PLACEMENT_3D('',#1573,#1212,#1213);
#966=AXIS2_PLACEMENT_3D('',#1574,#1214,#1215);
#967=AXIS2_PLACEMENT_3D('',#1575,#1216,#1217);
#968=AXIS2_PLACEMENT_3D('',#1576,#1218,#1219);
#969=AXIS2_PLACEMENT_3D('',#1577,#1220,#1221);
#970=AXIS2_PLACEMENT_3D('',#1578,#1222,#1223);
#971=AXIS2_PLACEMENT_3D('',#1579,#1224,#1225);
#972=AXIS2_PLACEMENT_3D('',#1580,#1226,#1227);
#973=AXIS2_PLACEMENT_3D('',#1581,#1228,#1229);
#974=AXIS2_PLACEMENT_3D('',#1582,#1230,#1231);
#975=DIRECTION('axis',(0.,0.,1.));
#976=DIRECTION('refdir',(1.,0.,0.));
#977=DIRECTION('axis',(0.,0.,1.));
#978=DIRECTION('refdir',(1.,0.,0.));
#979=DIRECTION('center_axis',(0.707106813733351,0.,0.707106748639742));
#980=DIRECTION('ref_axis',(0.707106748639742,0.,-0.707106813733351));
#981=DIRECTION('',(-0.707106748639742,0.,0.707106813733351));
#982=DIRECTION('',(0.,1.,0.));
#983=DIRECTION('',(-0.707106748639742,0.,0.707106813733351));
#984=DIRECTION('',(0.,-1.,0.));
#985=DIRECTION('center_axis',(0.,-1.,0.));
#986=DIRECTION('ref_axis',(1.,0.,0.));
#987=DIRECTION('center_axis',(0.,-1.,0.));
#988=DIRECTION('ref_axis',(1.,0.,0.));
#989=DIRECTION('',(0.,-1.,0.));
#990=DIRECTION('center_axis',(0.,1.,0.));
#991=DIRECTION('ref_axis',(1.,0.,0.));
#992=DIRECTION('',(0.,-1.,0.));
#993=DIRECTION('center_axis',(-0.707106781186548,0.,0.707106781186547));
#994=DIRECTION('ref_axis',(-0.707106781186547,0.,-0.707106781186548));
#995=DIRECTION('',(0.707106781186547,0.,0.707106781186548));
#996=DIRECTION('',(-0.707106781186547,0.,-0.707106781186548));
#997=DIRECTION('',(0.,-1.,0.));
#998=DIRECTION('center_axis',(0.,-1.,0.));
#999=DIRECTION('ref_axis',(-0.707106781186549,0.,0.707106781186546));
#1000=DIRECTION('center_axis',(0.,-1.,0.));
#1001=DIRECTION('ref_axis',(-0.707106781186549,0.,0.707106781186546));
#1002=DIRECTION('center_axis',(0.,1.,0.));
#1003=DIRECTION('ref_axis',(-0.707106781186549,0.,0.707106781186546));
#1004=DIRECTION('',(0.,-1.,0.));
#1005=DIRECTION('center_axis',(0.707106781186548,0.,-0.707106781186548));
#1006=DIRECTION('ref_axis',(0.707106781186548,0.,0.707106781186548));
#1007=DIRECTION('',(-0.707106781186547,0.,-0.707106781186547));
#1008=DIRECTION('',(0.707106781186547,0.,0.707106781186547));
#1009=DIRECTION('',(0.,1.,0.));
#1010=DIRECTION('center_axis',(0.,-1.,0.));
#1011=DIRECTION('ref_axis',(1.,0.,0.));
#1012=DIRECTION('center_axis',(0.,-1.,0.));
#1013=DIRECTION('ref_axis',(1.,0.,0.));
#1014=DIRECTION('center_axis',(0.,-1.,0.));
#1015=DIRECTION('ref_axis',(0.579365558580642,0.,0.815067818976151));
#1016=DIRECTION('',(0.,-1.,0.));
#1017=DIRECTION('center_axis',(-0.707106781186548,0.,-0.707106781186547));
#1018=DIRECTION('ref_axis',(0.707106781186547,0.,-0.707106781186548));
#1019=DIRECTION('',(-0.707106781186547,0.,0.707106781186548));
#1020=DIRECTION('',(0.707106781186547,0.,-0.707106781186548));
#1021=DIRECTION('',(0.,-1.,0.));
#1022=DIRECTION('center_axis',(0.,-1.,0.));
#1023=DIRECTION('ref_axis',(-0.707106781186547,0.,-0.707106781186548));
#1024=DIRECTION('center_axis',(0.,-1.,0.));
#1025=DIRECTION('ref_axis',(-0.707106781186547,0.,-0.707106781186548));
#1026=DIRECTION('center_axis',(0.,1.,0.));
#1027=DIRECTION('ref_axis',(-0.707106781186547,0.,-0.707106781186548));
#1028=DIRECTION('',(0.,-1.,0.));
#1029=DIRECTION('center_axis',(0.707106781186548,0.,0.707106781186547));
#1030=DIRECTION('ref_axis',(-0.707106781186547,0.,0.707106781186548));
#1031=DIRECTION('',(0.707106781186547,0.,-0.707106781186548));
#1032=DIRECTION('',(-0.707106781186547,0.,0.707106781186548));
#1033=DIRECTION('',(0.,-1.,0.));
#1034=DIRECTION('center_axis',(0.,-1.,0.));
#1035=DIRECTION('ref_axis',(-1.,0.,1.22464679914735E-16));
#1036=DIRECTION('center_axis',(0.,-1.,0.));
#1037=DIRECTION('ref_axis',(1.,0.,0.));
#1038=DIRECTION('center_axis',(0.,1.,0.));
#1039=DIRECTION('ref_axis',(1.,0.,0.));
#1040=DIRECTION('',(0.,-1.,0.));
#1041=DIRECTION('center_axis',(0.707106781186547,0.,-0.707106781186548));
#1042=DIRECTION('ref_axis',(0.707106781186548,0.,0.707106781186547));
#1043=DIRECTION('',(-0.707106781186548,0.,-0.707106781186547));
#1044=DIRECTION('',(0.707106781186548,0.,0.707106781186547));
#1045=DIRECTION('',(0.,-1.,0.));
#1046=DIRECTION('center_axis',(0.,-1.,0.));
#1047=DIRECTION('ref_axis',(-0.707106786454903,0.,-0.707106775918192));
#1048=DIRECTION('center_axis',(0.,-1.,0.));
#1049=DIRECTION('ref_axis',(0.707106781186548,0.,-0.707106781186547));
#1050=DIRECTION('center_axis',(0.,1.,0.));
#1051=DIRECTION('ref_axis',(0.707106781186548,0.,-0.707106781186547));
#1052=DIRECTION('',(0.,-1.,0.));
#1053=DIRECTION('center_axis',(-0.707106781186547,0.,0.707106781186548));
#1054=DIRECTION('ref_axis',(-0.707106781186548,0.,-0.707106781186547));
#1055=DIRECTION('',(0.707106781186548,0.,0.707106781186547));
#1056=DIRECTION('',(-0.707106781186548,0.,-0.707106781186547));
#1057=DIRECTION('',(0.,-1.,0.));
#1058=DIRECTION('center_axis',(0.,-1.,0.));
#1059=DIRECTION('ref_axis',(1.,0.,0.));
#1060=DIRECTION('center_axis',(0.,-1.,0.));
#1061=DIRECTION('ref_axis',(1.,0.,0.));
#1062=DIRECTION('center_axis',(0.,1.,0.));
#1063=DIRECTION('ref_axis',(1.,0.,0.));
#1064=DIRECTION('center_axis',(0.707106781186548,0.,0.707106781186547));
#1065=DIRECTION('ref_axis',(-0.707106781186547,0.,0.707106781186548));
#1066=DIRECTION('',(0.707106781186547,0.,-0.707106781186548));
#1067=DIRECTION('',(-0.707106781186547,0.,0.707106781186548));
#1068=DIRECTION('',(0.,-1.,0.));
#1069=DIRECTION('center_axis',(0.,-1.,0.));
#1070=DIRECTION('ref_axis',(0.707106775918192,0.,-0.707106786454903));
#1071=DIRECTION('center_axis',(0.,-1.,0.));
#1072=DIRECTION('ref_axis',(0.707106781186547,0.,0.707106781186548));
#1073=DIRECTION('center_axis',(0.,1.,0.));
#1074=DIRECTION('ref_axis',(0.707106781186547,0.,0.707106781186548));
#1075=DIRECTION('',(0.,-1.,0.));
#1076=DIRECTION('center_axis',(-0.707106781186548,0.,-0.707106781186547));
#1077=DIRECTION('ref_axis',(0.707106781186547,0.,-0.707106781186548));
#1078=DIRECTION('',(-0.707106781186547,0.,0.707106781186548));
#1079=DIRECTION('',(0.707106781186547,0.,-0.707106781186548));
#1080=DIRECTION('center_axis',(0.,-1.,0.));
#1081=DIRECTION('ref_axis',(1.,0.,0.));
#1082=DIRECTION('center_axis',(0.,-1.,0.));
#1083=DIRECTION('ref_axis',(1.,0.,0.));
#1084=DIRECTION('',(0.,1.,0.));
#1085=DIRECTION('center_axis',(0.,1.,0.));
#1086=DIRECTION('ref_axis',(1.,0.,0.));
#1087=DIRECTION('center_axis',(0.,1.,0.));
#1088=DIRECTION('ref_axis',(1.,0.,0.));
#1089=DIRECTION('center_axis',(0.,1.,0.));
#1090=DIRECTION('ref_axis',(1.,0.,0.));
#1091=DIRECTION('axis',(0.,0.,1.));
#1092=DIRECTION('refdir',(1.,0.,0.));
#1093=DIRECTION('center_axis',(0.,0.,1.));
#1094=DIRECTION('ref_axis',(1.,0.,0.));
#1095=DIRECTION('center_axis',(0.,0.,-1.));
#1096=DIRECTION('ref_axis',(1.,0.,0.));
#1097=DIRECTION('center_axis',(0.,0.,1.));
#1098=DIRECTION('ref_axis',(1.,0.,0.));
#1099=DIRECTION('center_axis',(0.,0.,1.));
#1100=DIRECTION('ref_axis',(1.,0.,0.));
#1101=DIRECTION('',(0.,0.,-1.));
#1102=DIRECTION('center_axis',(0.,0.,1.));
#1103=DIRECTION('ref_axis',(1.,0.,0.));
#1104=DIRECTION('axis',(0.,0.,1.));
#1105=DIRECTION('refdir',(1.,0.,0.));
#1106=DIRECTION('center_axis',(0.,0.,1.));
#1107=DIRECTION('ref_axis',(1.,0.,0.));
#1108=DIRECTION('',(0.,0.,1.));
#1109=DIRECTION('center_axis',(0.,0.,1.));
#1110=DIRECTION('ref_axis',(1.,0.,0.));
#1111=DIRECTION('',(0.,0.,1.));
#1112=DIRECTION('center_axis',(0.,-1.,0.));
#1113=DIRECTION('ref_axis',(1.,0.,0.));
#1114=DIRECTION('center_axis',(0.,1.,0.));
#1115=DIRECTION('ref_axis',(1.,0.,0.));
#1116=DIRECTION('',(0.,-1.,0.));
#1117=DIRECTION('center_axis',(0.,1.,0.));
#1118=DIRECTION('ref_axis',(1.,0.,0.));
#1119=DIRECTION('center_axis',(0.,-1.,0.));
#1120=DIRECTION('ref_axis',(1.,0.,0.));
#1121=DIRECTION('center_axis',(0.,-1.,0.));
#1122=DIRECTION('ref_axis',(1.,0.,0.));
#1123=DIRECTION('',(0.,1.,0.));
#1124=DIRECTION('center_axis',(0.,-1.,0.));
#1125=DIRECTION('ref_axis',(1.,0.,0.));
#1126=DIRECTION('center_axis',(0.,-1.,0.));
#1127=DIRECTION('ref_axis',(1.,0.,0.));
#1128=DIRECTION('center_axis',(0.,-1.,0.));
#1129=DIRECTION('ref_axis',(1.,0.,0.));
#1130=DIRECTION('axis',(0.,0.,1.));
#1131=DIRECTION('refdir',(1.,0.,0.));
#1132=DIRECTION('center_axis',(0.,1.,0.));
#1133=DIRECTION('ref_axis',(1.,0.,0.));
#1134=DIRECTION('center_axis',(0.,-1.,0.));
#1135=DIRECTION('ref_axis',(1.,0.,0.));
#1136=DIRECTION('center_axis',(0.,-1.,0.));
#1137=DIRECTION('ref_axis',(1.,0.,0.));
#1138=DIRECTION('',(0.,1.,0.));
#1139=DIRECTION('center_axis',(0.,-1.,0.));
#1140=DIRECTION('ref_axis',(1.,0.,0.));
#1141=DIRECTION('center_axis',(0.,1.,0.));
#1142=DIRECTION('ref_axis',(1.,0.,0.));
#1143=DIRECTION('axis',(0.,0.,1.));
#1144=DIRECTION('refdir',(1.,0.,0.));
#1145=DIRECTION('center_axis',(0.,0.,1.));
#1146=DIRECTION('ref_axis',(1.,0.,0.));
#1147=DIRECTION('center_axis',(0.,0.,-1.));
#1148=DIRECTION('ref_axis',(1.,0.,0.));
#1149=DIRECTION('center_axis',(0.,0.,1.));
#1150=DIRECTION('ref_axis',(1.,0.,0.));
#1151=DIRECTION('center_axis',(0.,0.,1.));
#1152=DIRECTION('ref_axis',(1.,0.,0.));
#1153=DIRECTION('',(0.,0.,-1.));
#1154=DIRECTION('center_axis',(0.,0.,1.));
#1155=DIRECTION('ref_axis',(1.,0.,0.));
#1156=DIRECTION('axis',(0.,0.,1.));
#1157=DIRECTION('refdir',(1.,0.,0.));
#1158=DIRECTION('center_axis',(0.,1.,0.));
#1159=DIRECTION('ref_axis',(-1.,0.,0.));
#1160=DIRECTION('center_axis',(0.,1.,0.));
#1161=DIRECTION('ref_axis',(-1.,0.,0.));
#1162=DIRECTION('',(0.,1.,0.));
#1163=DIRECTION('center_axis',(0.,-1.,0.));
#1164=DIRECTION('ref_axis',(-1.,0.,0.));
#1165=DIRECTION('center_axis',(0.,-1.,0.));
#1166=DIRECTION('ref_axis',(1.,0.,0.));
#1167=DIRECTION('center_axis',(0.,-1.,0.));
#1168=DIRECTION('ref_axis',(1.,0.,0.));
#1169=DIRECTION('',(0.,-1.,0.));
#1170=DIRECTION('center_axis',(0.,1.,0.));
#1171=DIRECTION('ref_axis',(1.,0.,0.));
#1172=DIRECTION('center_axis',(0.,1.,0.));
#1173=DIRECTION('ref_axis',(1.,0.,0.));
#1174=DIRECTION('center_axis',(0.,1.,0.));
#1175=DIRECTION('ref_axis',(1.,0.,0.));
#1176=DIRECTION('',(0.,-1.,0.));
#1177=DIRECTION('center_axis',(0.,1.,0.));
#1178=DIRECTION('ref_axis',(1.,0.,0.));
#1179=DIRECTION('center_axis',(0.,1.,0.));
#1180=DIRECTION('ref_axis',(1.,0.,0.));
#1181=DIRECTION('center_axis',(0.,1.,0.));
#1182=DIRECTION('ref_axis',(1.,0.,0.));
#1183=DIRECTION('axis',(0.,0.,1.));
#1184=DIRECTION('refdir',(1.,0.,0.));
#1185=DIRECTION('center_axis',(0.,1.,0.));
#1186=DIRECTION('ref_axis',(-1.,0.,0.));
#1187=DIRECTION('center_axis',(0.,1.,0.));
#1188=DIRECTION('ref_axis',(-1.,0.,0.));
#1189=DIRECTION('',(0.,-1.,0.));
#1190=DIRECTION('center_axis',(0.,1.,0.));
#1191=DIRECTION('ref_axis',(-1.,0.,0.));
#1192=DIRECTION('center_axis',(0.,1.,0.));
#1193=DIRECTION('ref_axis',(-1.,0.,0.));
#1194=DIRECTION('center_axis',(0.,1.,0.));
#1195=DIRECTION('ref_axis',(-1.,0.,0.));
#1196=DIRECTION('axis',(0.,0.,1.));
#1197=DIRECTION('refdir',(1.,0.,0.));
#1198=DIRECTION('center_axis',(0.,-1.,0.));
#1199=DIRECTION('ref_axis',(1.,0.,0.));
#1200=DIRECTION('center_axis',(0.,1.,0.));
#1201=DIRECTION('ref_axis',(1.,0.,0.));
#1202=DIRECTION('',(0.,-1.,0.));
#1203=DIRECTION('center_axis',(0.,1.,0.));
#1204=DIRECTION('ref_axis',(1.,0.,0.));
#1205=DIRECTION('center_axis',(0.,-1.,0.));
#1206=DIRECTION('ref_axis',(1.,0.,0.));
#1207=DIRECTION('center_axis',(0.,-1.,0.));
#1208=DIRECTION('ref_axis',(1.,0.,0.));
#1209=DIRECTION('',(0.,1.,0.));
#1210=DIRECTION('center_axis',(0.,-1.,0.));
#1211=DIRECTION('ref_axis',(1.,0.,0.));
#1212=DIRECTION('center_axis',(0.,-1.,0.));
#1213=DIRECTION('ref_axis',(1.,0.,0.));
#1214=DIRECTION('center_axis',(0.,-1.,0.));
#1215=DIRECTION('ref_axis',(1.,0.,0.));
#1216=DIRECTION('',(0.,0.,1.));
#1217=DIRECTION('',(1.,0.,0.));
#1218=DIRECTION('',(0.,0.,1.));
#1219=DIRECTION('',(1.,0.,0.));
#1220=DIRECTION('',(0.,0.,1.));
#1221=DIRECTION('',(1.,0.,0.));
#1222=DIRECTION('',(0.,0.,1.));
#1223=DIRECTION('',(1.,0.,0.));
#1224=DIRECTION('',(0.,0.,1.));
#1225=DIRECTION('',(1.,0.,0.));
#1226=DIRECTION('',(0.,0.,1.));
#1227=DIRECTION('',(1.,0.,0.));
#1228=DIRECTION('',(0.,0.,1.));
#1229=DIRECTION('',(1.,0.,0.));
#1230=DIRECTION('',(0.,0.,1.));
#1231=DIRECTION('',(1.,0.,0.));
#1232=CARTESIAN_POINT('',(0.,0.,0.));
#1233=CARTESIAN_POINT('',(0.,0.,0.));
#1234=CARTESIAN_POINT('Origin',(10.4285802387844,-8.,35.3287793894565));
#1235=CARTESIAN_POINT('',(13.854312705131,-3.,31.9030466077497));
#1236=CARTESIAN_POINT('',(10.4285802387843,-3.,35.3287793894565));
#1237=CARTESIAN_POINT('',(7.10531883627285,-3.,38.6520410978951));
#1238=CARTESIAN_POINT('',(10.4285802387843,-8.,35.3287793894565));
#1239=CARTESIAN_POINT('',(10.4285802387843,-8.,35.3287793894565));
#1240=CARTESIAN_POINT('',(13.854312705131,-8.,31.9030466077497));
#1241=CARTESIAN_POINT('',(13.854312705131,-8.,31.9030466077497));
#1242=CARTESIAN_POINT('',(13.854312705131,-3.,31.9030466077497));
#1243=CARTESIAN_POINT('Origin',(0.,-3.,50.));
#1244=CARTESIAN_POINT('',(14.6712207415708,-3.,39.5714199455485));
#1245=CARTESIAN_POINT('',(14.6712207415708,-3.,60.4285800544515));
#1246=CARTESIAN_POINT('Origin',(0.,-3.,50.));
#1247=CARTESIAN_POINT('',(14.6712207415708,-8.,39.5714199455485));
#1248=CARTESIAN_POINT('',(14.6712207415708,-3.,39.5714199455485));
#1249=CARTESIAN_POINT('',(14.6712207415708,-8.,60.4285800544515));
#1250=CARTESIAN_POINT('Origin',(0.,-8.,50.));
#1251=CARTESIAN_POINT('',(14.6712207415708,-3.,60.4285800544515));
#1252=CARTESIAN_POINT('Origin',(29.3122930478506,-3.,75.0696523607313));
#1253=CARTESIAN_POINT('',(29.3122930478506,-3.,75.0696523607313));
#1254=CARTESIAN_POINT('',(29.3122930478506,-3.,75.0696523607313));
#1255=CARTESIAN_POINT('',(29.3122930478506,-8.,75.0696523607313));
#1256=CARTESIAN_POINT('',(29.3122930478506,-8.,75.0696523607313));
#1257=CARTESIAN_POINT('',(29.3122930478506,-3.,75.0696523607313));
#1258=CARTESIAN_POINT('Origin',(27.190972704291,-3.,77.190972704291));
#1259=CARTESIAN_POINT('',(25.0696523607313,-3.,79.3122930478506));
#1260=CARTESIAN_POINT('Origin',(27.190972704291,-3.,77.190972704291));
#1261=CARTESIAN_POINT('',(25.0696523607313,-8.,79.3122930478506));
#1262=CARTESIAN_POINT('Origin',(27.190972704291,-8.,77.190972704291));
#1263=CARTESIAN_POINT('',(25.0696523607313,-3.,79.3122930478506));
#1264=CARTESIAN_POINT('Origin',(13.854312705131,-3.,68.0969533922503));
#1265=CARTESIAN_POINT('',(10.4285800544516,-3.,64.6712207415707));
#1266=CARTESIAN_POINT('',(6.12338976254612,-3.,60.3660304496654));
#1267=CARTESIAN_POINT('',(10.4285800544516,-8.,64.6712207415707));
#1268=CARTESIAN_POINT('',(6.12338976254612,-8.,60.3660304496654));
#1269=CARTESIAN_POINT('',(10.4285800544516,-8.,64.6712207415707));
#1270=CARTESIAN_POINT('Origin',(0.,-3.,50.));
#1271=CARTESIAN_POINT('',(-10.4285800544515,-3.,64.6712207415708));
#1272=CARTESIAN_POINT('Origin',(0.,-3.,50.));
#1273=CARTESIAN_POINT('',(-10.4285800544515,-8.,64.6712207415708));
#1274=CARTESIAN_POINT('Origin',(0.,-8.,50.));
#1275=CARTESIAN_POINT('',(-10.4285800544515,-3.,64.6712207415708));
#1276=CARTESIAN_POINT('Origin',(-25.0696523607313,-3.,79.3122930478506));
#1277=CARTESIAN_POINT('',(-25.0696523923415,-3.,79.3122930794607));
#1278=CARTESIAN_POINT('',(-25.0696523607313,-3.,79.3122930478506));
#1279=CARTESIAN_POINT('',(-25.0696523923415,-8.,79.3122930794608));
#1280=CARTESIAN_POINT('',(-25.0696523607313,-8.,79.3122930478506));
#1281=CARTESIAN_POINT('',(-25.0696523923415,-3.,79.3122930794607));
#1282=CARTESIAN_POINT('Origin',(-27.190972704291,-3.,77.190972704291));
#1283=CARTESIAN_POINT('',(-29.3122930478506,-3.,75.0696523607313));
#1284=CARTESIAN_POINT('Origin',(-27.190972704291,-3.,77.190972704291));
#1285=CARTESIAN_POINT('',(-29.3122930478506,-8.,75.0696523607313));
#1286=CARTESIAN_POINT('Origin',(-27.190972704291,-8.,77.190972704291));
#1287=CARTESIAN_POINT('',(-29.3122930478506,-3.,75.0696523607313));
#1288=CARTESIAN_POINT('Origin',(-14.6712207415708,-3.,60.4285800544515));
#1289=CARTESIAN_POINT('',(-14.6712207415708,-3.,60.4285800544515));
#1290=CARTESIAN_POINT('',(-10.3660304496654,-3.,56.1233897625461));
#1291=CARTESIAN_POINT('',(-14.6712207415708,-8.,60.4285800544515));
#1292=CARTESIAN_POINT('',(-10.3660304496654,-8.,56.1233897625461));
#1293=CARTESIAN_POINT('',(-14.6712207415708,-3.,60.4285800544515));
#1294=CARTESIAN_POINT('Origin',(0.,-3.,50.));
#1295=CARTESIAN_POINT('',(-14.6712207415708,-3.,39.5714199455485));
#1296=CARTESIAN_POINT('Origin',(0.,-3.,50.));
#1297=CARTESIAN_POINT('',(-14.6712207415708,-8.,39.5714199455485));
#1298=CARTESIAN_POINT('Origin',(0.,-8.,50.));
#1299=CARTESIAN_POINT('',(-14.6712207415708,-3.,39.5714199455485));
#1300=CARTESIAN_POINT('Origin',(-29.3122930162405,-3.,24.9303476708788));
#1301=CARTESIAN_POINT('',(-29.3122930162405,-3.,24.9303476708788));
#1302=CARTESIAN_POINT('',(-29.3122930478506,-3.,24.9303476392687));
#1303=CARTESIAN_POINT('',(-29.3122930162405,-8.,24.9303476708788));
#1304=CARTESIAN_POINT('',(-29.3122930478506,-8.,24.9303476392687));
#1305=CARTESIAN_POINT('',(-29.3122930162405,-3.,24.9303476708788));
#1306=CARTESIAN_POINT('Origin',(-27.190972704291,-3.,22.809027295709));
#1307=CARTESIAN_POINT('',(-25.0696523607313,-3.,20.6877069521494));
#1308=CARTESIAN_POINT('Origin',(-27.190972704291,-3.,22.809027295709));
#1309=CARTESIAN_POINT('',(-25.0696523607313,-8.,20.6877069521494));
#1310=CARTESIAN_POINT('Origin',(-27.190972704291,-8.,22.809027295709));
#1311=CARTESIAN_POINT('',(-25.0696523607313,-3.,20.6877069521494));
#1312=CARTESIAN_POINT('Origin',(-10.4285800544515,-3.,35.3287792584292));
#1313=CARTESIAN_POINT('',(-10.4285800544515,-3.,35.3287792584292));
#1314=CARTESIAN_POINT('',(-6.12338976254612,-3.,39.6339695503346));
#1315=CARTESIAN_POINT('',(-10.4285800544515,-8.,35.3287792584292));
#1316=CARTESIAN_POINT('',(-6.12338976254612,-8.,39.6339695503346));
#1317=CARTESIAN_POINT('',(-10.4285800544515,-3.,35.3287792584292));
#1318=CARTESIAN_POINT('Origin',(0.,-3.,50.));
#1319=CARTESIAN_POINT('Origin',(0.,-3.,50.));
#1320=CARTESIAN_POINT('Origin',(0.,-8.,50.));
#1321=CARTESIAN_POINT('Origin',(25.0696523291212,-3.,20.6877069837595));
#1322=CARTESIAN_POINT('',(25.0696523291212,-3.,20.6877069837595));
#1323=CARTESIAN_POINT('',(25.0696523607313,-3.,20.6877069521494));
#1324=CARTESIAN_POINT('',(25.0696523291212,-8.,20.6877069837595));
#1325=CARTESIAN_POINT('',(25.0696523607313,-8.,20.6877069521494));
#1326=CARTESIAN_POINT('',(25.0696523291212,-3.,20.6877069837595));
#1327=CARTESIAN_POINT('Origin',(27.190972704291,-3.,22.809027295709));
#1328=CARTESIAN_POINT('',(29.3122930478506,-3.,24.9303476392687));
#1329=CARTESIAN_POINT('Origin',(27.190972704291,-3.,22.809027295709));
#1330=CARTESIAN_POINT('',(29.3122930478506,-8.,24.9303476392687));
#1331=CARTESIAN_POINT('Origin',(27.190972704291,-8.,22.809027295709));
#1332=CARTESIAN_POINT('',(29.3122930478506,-3.,24.9303476392687));
#1333=CARTESIAN_POINT('Origin',(14.6712207415708,-3.,39.5714199455485));
#1334=CARTESIAN_POINT('',(10.3660304496654,-3.,43.8766102374539));
#1335=CARTESIAN_POINT('',(10.3660304496654,-8.,43.8766102374539));
#1336=CARTESIAN_POINT('Origin',(0.,-3.,50.));
#1337=CARTESIAN_POINT('',(-47.,-8.,50.));
#1338=CARTESIAN_POINT('Origin',(0.,-8.,50.));
#1339=CARTESIAN_POINT('',(-47.,-3.,50.));
#1340=CARTESIAN_POINT('',(-47.,-3.,50.));
#1341=CARTESIAN_POINT('Origin',(0.,-3.,50.));
#1342=CARTESIAN_POINT('Origin',(0.,-3.,50.));
#1343=CARTESIAN_POINT('Origin',(0.,-8.,50.));
#1344=CARTESIAN_POINT('',(0.,0.,0.));
#1345=CARTESIAN_POINT('Origin',(0.,0.,-2.));
#1346=CARTESIAN_POINT('',(-2.5,-3.06161699786838E-16,-2.));
#1347=CARTESIAN_POINT('Origin',(0.,0.,-2.));
#1348=CARTESIAN_POINT('Origin',(0.,0.,0.));
#1349=CARTESIAN_POINT('',(-2.5,-3.06161699786838E-16,5.5));
#1350=CARTESIAN_POINT('Origin',(0.,0.,5.5));
#1351=CARTESIAN_POINT('',(-2.5,-3.06161699786838E-16,0.));
#1352=CARTESIAN_POINT('Origin',(0.,0.,5.5));
#1353=CARTESIAN_POINT('',(0.,0.,0.));
#1354=CARTESIAN_POINT('Origin',(0.,0.,0.));
#1355=CARTESIAN_POINT('',(-2.5,-6.93889390390723E-17,2.06514837824155));
#1356=CARTESIAN_POINT('Ctrl Pts',(-2.5,0.,2.06514837824153));
#1357=CARTESIAN_POINT('Ctrl Pts',(-2.5,-0.313966549966975,2.06514837824153));
#1358=CARTESIAN_POINT('Ctrl Pts',(-2.43724208175823,-0.648821661237632,
2.06174633522331));
#1359=CARTESIAN_POINT('Ctrl Pts',(-2.18209026124743,-1.26475318832061,2.04945469062714));
#1360=CARTESIAN_POINT('Ctrl Pts',(-1.98969948627882,-1.54583441965392,2.04074211479646));
#1361=CARTESIAN_POINT('Ctrl Pts',(-1.54583447486274,-1.98969943106999,2.02438414468301));
#1362=CARTESIAN_POINT('Ctrl Pts',(-1.26475321841524,-2.18209024745813,2.0156767273781));
#1363=CARTESIAN_POINT('Ctrl Pts',(-0.648821611717717,-2.43724210359452,
2.00339687904366));
#1364=CARTESIAN_POINT('Ctrl Pts',(-0.313966471863397,-2.5,1.99999999999999));
#1365=CARTESIAN_POINT('Ctrl Pts',(0.313966471863396,-2.5,1.99999999999999));
#1366=CARTESIAN_POINT('Ctrl Pts',(0.648821611717716,-2.43724210359452,2.00339687904366));
#1367=CARTESIAN_POINT('Ctrl Pts',(1.26475321841524,-2.18209024745813,2.0156767273781));
#1368=CARTESIAN_POINT('Ctrl Pts',(1.54583447486274,-1.98969943106999,2.02438414468301));
#1369=CARTESIAN_POINT('Ctrl Pts',(1.98969948627882,-1.54583441965392,2.04074211479646));
#1370=CARTESIAN_POINT('Ctrl Pts',(2.18209026124743,-1.26475318832061,2.04945469062714));
#1371=CARTESIAN_POINT('Ctrl Pts',(2.43724208175823,-0.648821661237632,2.06174633522331));
#1372=CARTESIAN_POINT('Ctrl Pts',(2.5,-0.313966549966975,2.06514837824153));
#1373=CARTESIAN_POINT('Ctrl Pts',(2.5,0.313966549966975,2.06514837824153));
#1374=CARTESIAN_POINT('Ctrl Pts',(2.43724208175823,0.648821661237632,2.06174633522331));
#1375=CARTESIAN_POINT('Ctrl Pts',(2.18209026124743,1.26475318832061,2.04945469062714));
#1376=CARTESIAN_POINT('Ctrl Pts',(1.98969948627882,1.54583441965392,2.04074211479646));
#1377=CARTESIAN_POINT('Ctrl Pts',(1.54583447486274,1.98969943106999,2.02438414468301));
#1378=CARTESIAN_POINT('Ctrl Pts',(1.26475321841524,2.18209024745813,2.0156767273781));
#1379=CARTESIAN_POINT('Ctrl Pts',(0.648821611717718,2.43724210359452,2.00339687904366));
#1380=CARTESIAN_POINT('Ctrl Pts',(0.313966471863397,2.5,1.99999999999999));
#1381=CARTESIAN_POINT('Ctrl Pts',(-0.313966471863395,2.5,1.99999999999999));
#1382=CARTESIAN_POINT('Ctrl Pts',(-0.648821611717715,2.43724210359452,2.00339687904366));
#1383=CARTESIAN_POINT('Ctrl Pts',(-1.26475321841524,2.18209024745813,2.0156767273781));
#1384=CARTESIAN_POINT('Ctrl Pts',(-1.54583447486274,1.98969943107,2.02438414468301));
#1385=CARTESIAN_POINT('Ctrl Pts',(-1.98969948627882,1.54583441965392,2.04074211479646));
#1386=CARTESIAN_POINT('Ctrl Pts',(-2.18209026124743,1.26475318832061,2.04945469062714));
#1387=CARTESIAN_POINT('Ctrl Pts',(-2.43724208175823,0.648821661237633,2.06174633522331));
#1388=CARTESIAN_POINT('Ctrl Pts',(-2.5,0.313966549966975,2.06514837824153));
#1389=CARTESIAN_POINT('Ctrl Pts',(-2.5,-1.38777878078145E-16,2.06514837824153));
#1390=CARTESIAN_POINT('',(-2.5,-1.38777878078145E-16,5.06949811097144));
#1391=CARTESIAN_POINT('',(-2.5,-3.06161699786838E-16,0.));
#1392=CARTESIAN_POINT('Ctrl Pts',(-2.5,-2.08166817117217E-16,5.06949811097143));
#1393=CARTESIAN_POINT('Ctrl Pts',(-2.5,0.31397496870802,5.06949811097143));
#1394=CARTESIAN_POINT('Ctrl Pts',(-2.43723879407712,0.648833697924306,5.06586836285142));
#1395=CARTESIAN_POINT('Ctrl Pts',(-2.18208453863604,1.26476290215938,5.05275507922167));
#1396=CARTESIAN_POINT('Ctrl Pts',(-1.98969504628277,1.54583885964997,5.04346052213127));
#1397=CARTESIAN_POINT('Ctrl Pts',(-1.54583893114345,1.98969497478929,5.02601073765469));
#1398=CARTESIAN_POINT('Ctrl Pts',(-1.26476294130742,2.18208452114785,5.01672244237508));
#1399=CARTESIAN_POINT('Ctrl Pts',(-0.64883363366083,2.4372388219696,5.00362347878181));
#1400=CARTESIAN_POINT('Ctrl Pts',(-0.313974867561901,2.5,5.));
#1401=CARTESIAN_POINT('Ctrl Pts',(0.313974867561902,2.5,5.));
#1402=CARTESIAN_POINT('Ctrl Pts',(0.648833633660831,2.4372388219696,5.00362347878181));
#1403=CARTESIAN_POINT('Ctrl Pts',(1.26476294130743,2.18208452114784,5.01672244237508));
#1404=CARTESIAN_POINT('Ctrl Pts',(1.54583893114345,1.98969497478929,5.02601073765469));
#1405=CARTESIAN_POINT('Ctrl Pts',(1.98969504628277,1.54583885964996,5.04346052213127));
#1406=CARTESIAN_POINT('Ctrl Pts',(2.18208453863604,1.26476290215938,5.05275507922167));
#1407=CARTESIAN_POINT('Ctrl Pts',(2.43723879407712,0.648833697924305,5.06586836285142));
#1408=CARTESIAN_POINT('Ctrl Pts',(2.5,0.31397496870802,5.06949811097143));
#1409=CARTESIAN_POINT('Ctrl Pts',(2.5,-0.31397496870802,5.06949811097143));
#1410=CARTESIAN_POINT('Ctrl Pts',(2.43723879407712,-0.648833697924305,5.06586836285142));
#1411=CARTESIAN_POINT('Ctrl Pts',(2.18208453863604,-1.26476290215938,5.05275507922167));
#1412=CARTESIAN_POINT('Ctrl Pts',(1.98969504628277,-1.54583885964996,5.04346052213127));
#1413=CARTESIAN_POINT('Ctrl Pts',(1.54583893114345,-1.98969497478929,5.02601073765469));
#1414=CARTESIAN_POINT('Ctrl Pts',(1.26476294130743,-2.18208452114784,5.01672244237508));
#1415=CARTESIAN_POINT('Ctrl Pts',(0.648833633660831,-2.4372388219696,5.00362347878181));
#1416=CARTESIAN_POINT('Ctrl Pts',(0.313974867561901,-2.5,5.));
#1417=CARTESIAN_POINT('Ctrl Pts',(-0.313974867561902,-2.5,5.));
#1418=CARTESIAN_POINT('Ctrl Pts',(-0.648833633660832,-2.4372388219696,5.00362347878181));
#1419=CARTESIAN_POINT('Ctrl Pts',(-1.26476294130743,-2.18208452114784,5.01672244237508));
#1420=CARTESIAN_POINT('Ctrl Pts',(-1.54583893114345,-1.98969497478929,5.02601073765469));
#1421=CARTESIAN_POINT('Ctrl Pts',(-1.98969504628277,-1.54583885964996,5.04346052213127));
#1422=CARTESIAN_POINT('Ctrl Pts',(-2.18208453863604,-1.26476290215938,5.05275507922167));
#1423=CARTESIAN_POINT('Ctrl Pts',(-2.43723879407712,-0.648833697924305,
5.06586836285142));
#1424=CARTESIAN_POINT('Ctrl Pts',(-2.5,-0.31397496870802,5.06949811097143));
#1425=CARTESIAN_POINT('Ctrl Pts',(-2.5,6.93889390390723E-17,5.06949811097143));
#1426=CARTESIAN_POINT('Origin',(0.,0.,96.6));
#1427=CARTESIAN_POINT('',(-2.5,6.93889390390723E-17,94.9305018890286));
#1428=CARTESIAN_POINT('Ctrl Pts',(-2.5,1.38777878078145E-16,94.9305018890286));
#1429=CARTESIAN_POINT('Ctrl Pts',(-2.5,-0.31397496870802,94.9305018890286));
#1430=CARTESIAN_POINT('Ctrl Pts',(-2.43723879407712,-0.648833697924305,
94.9341316371486));
#1431=CARTESIAN_POINT('Ctrl Pts',(-2.18208453863604,-1.26476290215938,94.9472449207783));
#1432=CARTESIAN_POINT('Ctrl Pts',(-1.98969504628277,-1.54583885964996,94.9565394778687));
#1433=CARTESIAN_POINT('Ctrl Pts',(-1.54583893114345,-1.98969497478929,94.9739892623453));
#1434=CARTESIAN_POINT('Ctrl Pts',(-1.26476294130743,-2.18208452114784,94.9832775576249));
#1435=CARTESIAN_POINT('Ctrl Pts',(-0.648833633660833,-2.4372388219696,94.9963765212182));
#1436=CARTESIAN_POINT('Ctrl Pts',(-0.313974867561903,-2.5,95.));
#1437=CARTESIAN_POINT('Ctrl Pts',(0.313974867561902,-2.5,95.));
#1438=CARTESIAN_POINT('Ctrl Pts',(0.648833633660832,-2.4372388219696,94.9963765212182));
#1439=CARTESIAN_POINT('Ctrl Pts',(1.26476294130743,-2.18208452114784,94.9832775576249));
#1440=CARTESIAN_POINT('Ctrl Pts',(1.54583893114345,-1.98969497478929,94.9739892623453));
#1441=CARTESIAN_POINT('Ctrl Pts',(1.98969504628277,-1.54583885964996,94.9565394778687));
#1442=CARTESIAN_POINT('Ctrl Pts',(2.18208453863604,-1.26476290215938,94.9472449207783));
#1443=CARTESIAN_POINT('Ctrl Pts',(2.43723879407712,-0.648833697924305,94.9341316371486));
#1444=CARTESIAN_POINT('Ctrl Pts',(2.5,-0.31397496870802,94.9305018890286));
#1445=CARTESIAN_POINT('Ctrl Pts',(2.5,0.31397496870802,94.9305018890286));
#1446=CARTESIAN_POINT('Ctrl Pts',(2.43723879407712,0.648833697924305,94.9341316371486));
#1447=CARTESIAN_POINT('Ctrl Pts',(2.18208453863604,1.26476290215938,94.9472449207783));
#1448=CARTESIAN_POINT('Ctrl Pts',(1.98969504628277,1.54583885964996,94.9565394778687));
#1449=CARTESIAN_POINT('Ctrl Pts',(1.54583893114345,1.98969497478929,94.9739892623453));
#1450=CARTESIAN_POINT('Ctrl Pts',(1.26476294130743,2.18208452114784,94.9832775576249));
#1451=CARTESIAN_POINT('Ctrl Pts',(0.648833633660832,2.4372388219696,94.9963765212182));
#1452=CARTESIAN_POINT('Ctrl Pts',(0.313974867561903,2.5,95.));
#1453=CARTESIAN_POINT('Ctrl Pts',(-0.313974867561901,2.5,95.));
#1454=CARTESIAN_POINT('Ctrl Pts',(-0.648833633660831,2.4372388219696,94.9963765212182));
#1455=CARTESIAN_POINT('Ctrl Pts',(-1.26476294130743,2.18208452114784,94.9832775576249));
#1456=CARTESIAN_POINT('Ctrl Pts',(-1.54583893114345,1.98969497478929,94.9739892623453));
#1457=CARTESIAN_POINT('Ctrl Pts',(-1.98969504628277,1.54583885964997,94.9565394778687));
#1458=CARTESIAN_POINT('Ctrl Pts',(-2.18208453863604,1.26476290215938,94.9472449207783));
#1459=CARTESIAN_POINT('Ctrl Pts',(-2.43723879407712,0.648833697924306,94.9341316371486));
#1460=CARTESIAN_POINT('Ctrl Pts',(-2.5,0.313974968708021,94.9305018890286));
#1461=CARTESIAN_POINT('Ctrl Pts',(-2.5,0.,94.9305018890286));
#1462=CARTESIAN_POINT('',(-2.5,-1.38777878078145E-16,97.9348516217584));
#1463=CARTESIAN_POINT('',(-2.5,-3.06161699786838E-16,96.6));
#1464=CARTESIAN_POINT('Ctrl Pts',(-2.5,0.,97.9348516217585));
#1465=CARTESIAN_POINT('Ctrl Pts',(-2.5,0.313966549966976,97.9348516217585));
#1466=CARTESIAN_POINT('Ctrl Pts',(-2.43724208175823,0.648821661237634,97.9382536647767));
#1467=CARTESIAN_POINT('Ctrl Pts',(-2.18209026124743,1.26475318832061,97.9505453093728));
#1468=CARTESIAN_POINT('Ctrl Pts',(-1.98969948627882,1.54583441965392,97.9592578852035));
#1469=CARTESIAN_POINT('Ctrl Pts',(-1.54583447486274,1.98969943107,97.975615855317));
#1470=CARTESIAN_POINT('Ctrl Pts',(-1.26475321841524,2.18209024745813,97.9843232726219));
#1471=CARTESIAN_POINT('Ctrl Pts',(-0.648821611717716,2.43724210359452,97.9966031209564));
#1472=CARTESIAN_POINT('Ctrl Pts',(-0.313966471863395,2.5,98.));
#1473=CARTESIAN_POINT('Ctrl Pts',(0.313966471863397,2.5,98.));
#1474=CARTESIAN_POINT('Ctrl Pts',(0.648821611717718,2.43724210359452,97.9966031209564));
#1475=CARTESIAN_POINT('Ctrl Pts',(1.26475321841524,2.18209024745813,97.9843232726219));
#1476=CARTESIAN_POINT('Ctrl Pts',(1.54583447486274,1.98969943106999,97.975615855317));
#1477=CARTESIAN_POINT('Ctrl Pts',(1.98969948627882,1.54583441965392,97.9592578852035));
#1478=CARTESIAN_POINT('Ctrl Pts',(2.18209026124743,1.26475318832061,97.9505453093728));
#1479=CARTESIAN_POINT('Ctrl Pts',(2.43724208175823,0.648821661237632,97.9382536647767));
#1480=CARTESIAN_POINT('Ctrl Pts',(2.5,0.313966549966975,97.9348516217585));
#1481=CARTESIAN_POINT('Ctrl Pts',(2.5,-0.313966549966975,97.9348516217585));
#1482=CARTESIAN_POINT('Ctrl Pts',(2.43724208175823,-0.648821661237632,97.9382536647767));
#1483=CARTESIAN_POINT('Ctrl Pts',(2.18209026124743,-1.26475318832061,97.9505453093728));
#1484=CARTESIAN_POINT('Ctrl Pts',(1.98969948627882,-1.54583441965392,97.9592578852035));
#1485=CARTESIAN_POINT('Ctrl Pts',(1.54583447486274,-1.98969943106999,97.975615855317));
#1486=CARTESIAN_POINT('Ctrl Pts',(1.26475321841524,-2.18209024745813,97.9843232726219));
#1487=CARTESIAN_POINT('Ctrl Pts',(0.648821611717717,-2.43724210359452,97.9966031209564));
#1488=CARTESIAN_POINT('Ctrl Pts',(0.313966471863396,-2.5,98.));
#1489=CARTESIAN_POINT('Ctrl Pts',(-0.313966471863397,-2.5,98.));
#1490=CARTESIAN_POINT('Ctrl Pts',(-0.648821611717717,-2.43724210359452,
97.9966031209564));
#1491=CARTESIAN_POINT('Ctrl Pts',(-1.26475321841524,-2.18209024745813,97.9843232726219));
#1492=CARTESIAN_POINT('Ctrl Pts',(-1.54583447486274,-1.98969943106999,97.975615855317));
#1493=CARTESIAN_POINT('Ctrl Pts',(-1.98969948627882,-1.54583441965392,97.9592578852035));
#1494=CARTESIAN_POINT('Ctrl Pts',(-2.18209026124743,-1.26475318832061,97.9505453093728));
#1495=CARTESIAN_POINT('Ctrl Pts',(-2.43724208175823,-0.648821661237633,
97.9382536647767));
#1496=CARTESIAN_POINT('Ctrl Pts',(-2.5,-0.313966549966975,97.9348516217585));
#1497=CARTESIAN_POINT('Ctrl Pts',(-2.5,1.38777878078145E-16,97.9348516217585));
#1498=CARTESIAN_POINT('Origin',(0.,4.,50.));
#1499=CARTESIAN_POINT('',(-45.,4.,50.));
#1500=CARTESIAN_POINT('Origin',(0.,4.,50.));
#1501=CARTESIAN_POINT('',(-45.,-3.,50.));
#1502=CARTESIAN_POINT('',(-45.,4.,50.));
#1503=CARTESIAN_POINT('Origin',(0.,-3.,50.));
#1504=CARTESIAN_POINT('Origin',(0.,4.,50.));
#1505=CARTESIAN_POINT('',(-48.,-3.,50.));
#1506=CARTESIAN_POINT('Origin',(0.,-3.,50.));
#1507=CARTESIAN_POINT('',(-48.,4.,50.));
#1508=CARTESIAN_POINT('',(-48.,4.,50.));
#1509=CARTESIAN_POINT('Origin',(0.,4.,50.));
#1510=CARTESIAN_POINT('Origin',(0.,-3.,50.));
#1511=CARTESIAN_POINT('Origin',(0.,4.,50.));
#1512=CARTESIAN_POINT('',(0.,0.,0.));
#1513=CARTESIAN_POINT('Origin',(11.9313937448893,-8.,61.9313937448893));
#1514=CARTESIAN_POINT('',(9.43139374488932,-8.,61.9313937448893));
#1515=CARTESIAN_POINT('Origin',(11.9313937448893,-8.,61.9313937448893));
#1516=CARTESIAN_POINT('Origin',(11.9313937448893,-3.,61.9313937448893));
#1517=CARTESIAN_POINT('',(9.43139374488932,0.,61.9313937448893));
#1518=CARTESIAN_POINT('',(9.4313937448893,-3.,61.9313937448893));
#1519=CARTESIAN_POINT('Origin',(11.9313937448893,0.,61.9313937448893));
#1520=CARTESIAN_POINT('Origin',(23.8627874897787,0.,50.));
#1521=CARTESIAN_POINT('',(0.,0.,0.));
#1522=CARTESIAN_POINT('Origin',(0.,0.,94.6));
#1523=CARTESIAN_POINT('',(-2.5,-3.06161699786838E-16,94.6));
#1524=CARTESIAN_POINT('Origin',(0.,0.,94.6));
#1525=CARTESIAN_POINT('Origin',(0.,0.,96.6));
#1526=CARTESIAN_POINT('',(-2.5,-3.06161699786838E-16,102.1));
#1527=CARTESIAN_POINT('Origin',(0.,0.,102.1));
#1528=CARTESIAN_POINT('',(-2.5,-3.06161699786838E-16,96.6));
#1529=CARTESIAN_POINT('Origin',(0.,0.,102.1));
#1530=CARTESIAN_POINT('',(0.,0.,0.));
#1531=CARTESIAN_POINT('Origin',(23.8627874897787,0.,50.));
#1532=CARTESIAN_POINT('',(27.8627874897787,-3.,50.));
#1533=CARTESIAN_POINT('Origin',(23.8627874897787,-3.,50.));
#1534=CARTESIAN_POINT('',(27.8627874897787,0.,50.));
#1535=CARTESIAN_POINT('',(27.8627874897787,0.,50.));
#1536=CARTESIAN_POINT('Origin',(23.8627874897787,0.,50.));
#1537=CARTESIAN_POINT('Origin',(11.9313937448893,-3.,61.9313937448893));
#1538=CARTESIAN_POINT('',(9.43139374488932,0.,61.9313937448893));
#1539=CARTESIAN_POINT('Origin',(11.9313937448893,0.,61.9313937448893));
#1540=CARTESIAN_POINT('',(9.43139374488932,-3.,61.9313937448893));
#1541=CARTESIAN_POINT('',(9.4313937448893,-3.,61.9313937448893));
#1542=CARTESIAN_POINT('Origin',(11.9313937448893,-3.,61.9313937448893));
#1543=CARTESIAN_POINT('Origin',(23.8627874897787,-3.,50.));
#1544=CARTESIAN_POINT('',(3.18262091413893,0.,50.));
#1545=CARTESIAN_POINT('Origin',(23.8627874897787,0.,50.));
#1546=CARTESIAN_POINT('',(3.18262091413893,-3.,50.));
#1547=CARTESIAN_POINT('',(3.182620914139,-3.,50.));
#1548=CARTESIAN_POINT('Origin',(23.8627874897787,-3.,50.));
#1549=CARTESIAN_POINT('Origin',(23.8627874897787,0.,50.));
#1550=CARTESIAN_POINT('Origin',(23.8627874897787,-3.,50.));
#1551=CARTESIAN_POINT('',(0.,0.,0.));
#1552=CARTESIAN_POINT('Origin',(23.8627874897787,0.,50.));
#1553=CARTESIAN_POINT('',(27.8627874897787,5.9999998808,50.));
#1554=CARTESIAN_POINT('Origin',(23.8627874897787,5.9999998808,50.));
#1555=CARTESIAN_POINT('',(27.8627874897787,-3.,50.));
#1556=CARTESIAN_POINT('',(27.8627874897787,0.,50.));
#1557=CARTESIAN_POINT('Origin',(23.8627874897787,-3.,50.));
#1558=CARTESIAN_POINT('Origin',(23.8627874897787,5.9999998808,50.));
#1559=CARTESIAN_POINT('Origin',(23.8627874897787,-3.,50.));
#1560=CARTESIAN_POINT('',(0.,0.,0.));
#1561=CARTESIAN_POINT('Origin',(23.8627874897787,4.,50.));
#1562=CARTESIAN_POINT('',(19.8627874897787,4.,50.));
#1563=CARTESIAN_POINT('Origin',(23.8627874897787,4.,50.));
#1564=CARTESIAN_POINT('',(19.8627874897787,5.55111512312578E-16,50.));
#1565=CARTESIAN_POINT('',(19.8627874897787,4.,50.));
#1566=CARTESIAN_POINT('Origin',(23.8627874897787,5.55111512312578E-16,50.));
#1567=CARTESIAN_POINT('Origin',(23.8627874897787,4.,50.));
#1568=CARTESIAN_POINT('',(18.8627874897787,5.55111512312578E-16,50.));
#1569=CARTESIAN_POINT('Origin',(23.8627874897787,5.55111512312578E-16,50.));
#1570=CARTESIAN_POINT('',(18.8627874897787,4.,50.));
#1571=CARTESIAN_POINT('',(18.8627874897787,4.,50.));
#1572=CARTESIAN_POINT('Origin',(23.8627874897787,4.,50.));
#1573=CARTESIAN_POINT('Origin',(23.8627874897787,5.55111512312578E-16,50.));
#1574=CARTESIAN_POINT('Origin',(23.8627874897787,4.,50.));
#1575=CARTESIAN_POINT('',(0.,0.,0.));
#1576=CARTESIAN_POINT('',(0.,0.,0.));
#1577=CARTESIAN_POINT('',(0.,0.,0.));
#1578=CARTESIAN_POINT('',(0.,0.,0.));
#1579=CARTESIAN_POINT('',(0.,0.,0.));
#1580=CARTESIAN_POINT('',(0.,0.,0.));
#1581=CARTESIAN_POINT('',(0.,0.,0.));
#1582=CARTESIAN_POINT('',(0.,0.,0.));
#1583=UNCERTAINTY_MEASURE_WITH_UNIT(LENGTH_MEASURE(0.01),#1603,
'DISTANCE_ACCURACY_VALUE',
'Maximum model space distance between geometric entities at asserted c
onnectivities');
#1584=UNCERTAINTY_MEASURE_WITH_UNIT(LENGTH_MEASURE(0.01),#1603,
'DISTANCE_ACCURACY_VALUE',
'Maximum model space distance between geometric entities at asserted c
onnectivities');
#1585=UNCERTAINTY_MEASURE_WITH_UNIT(LENGTH_MEASURE(0.01),#1603,
'DISTANCE_ACCURACY_VALUE',
'Maximum model space distance between geometric entities at asserted c
onnectivities');
#1586=UNCERTAINTY_MEASURE_WITH_UNIT(LENGTH_MEASURE(0.01),#1603,
'DISTANCE_ACCURACY_VALUE',
'Maximum model space distance between geometric entities at asserted c
onnectivities');
#1587=UNCERTAINTY_MEASURE_WITH_UNIT(LENGTH_MEASURE(0.01),#1603,
'DISTANCE_ACCURACY_VALUE',
'Maximum model space distance between geometric entities at asserted c
onnectivities');
#1588=UNCERTAINTY_MEASURE_WITH_UNIT(LENGTH_MEASURE(0.01),#1603,
'DISTANCE_ACCURACY_VALUE',
'Maximum model space distance between geometric entities at asserted c
onnectivities');
#1589=UNCERTAINTY_MEASURE_WITH_UNIT(LENGTH_MEASURE(0.01),#1603,
'DISTANCE_ACCURACY_VALUE',
'Maximum model space distance between geometric entities at asserted c
onnectivities');
#1590=UNCERTAINTY_MEASURE_WITH_UNIT(LENGTH_MEASURE(0.01),#1603,
'DISTANCE_ACCURACY_VALUE',
'Maximum model space distance between geometric entities at asserted c
onnectivities');
#1591=UNCERTAINTY_MEASURE_WITH_UNIT(LENGTH_MEASURE(0.01),#1603,
'DISTANCE_ACCURACY_VALUE',
'Maximum model space distance between geometric entities at asserted c
onnectivities');
#1592=UNCERTAINTY_MEASURE_WITH_UNIT(LENGTH_MEASURE(0.01),#1603,
'DISTANCE_ACCURACY_VALUE',
'Maximum model space distance between geometric entities at asserted c
onnectivities');
#1593=(
GEOMETRIC_REPRESENTATION_CONTEXT(3)
GLOBAL_UNCERTAINTY_ASSIGNED_CONTEXT((#1583))
GLOBAL_UNIT_ASSIGNED_CONTEXT((#1603,#1605,#1606))
REPRESENTATION_CONTEXT('','3D')
);
#1594=(
GEOMETRIC_REPRESENTATION_CONTEXT(3)
GLOBAL_UNCERTAINTY_ASSIGNED_CONTEXT((#1584))
GLOBAL_UNIT_ASSIGNED_CONTEXT((#1603,#1605,#1606))
REPRESENTATION_CONTEXT('','3D')
);
#1595=(
GEOMETRIC_REPRESENTATION_CONTEXT(3)
GLOBAL_UNCERTAINTY_ASSIGNED_CONTEXT((#1585))
GLOBAL_UNIT_ASSIGNED_CONTEXT((#1603,#1605,#1606))
REPRESENTATION_CONTEXT('','3D')
);
#1596=(
GEOMETRIC_REPRESENTATION_CONTEXT(3)
GLOBAL_UNCERTAINTY_ASSIGNED_CONTEXT((#1586))
GLOBAL_UNIT_ASSIGNED_CONTEXT((#1603,#1605,#1606))
REPRESENTATION_CONTEXT('','3D')
);
#1597=(
GEOMETRIC_REPRESENTATION_CONTEXT(3)
GLOBAL_UNCERTAINTY_ASSIGNED_CONTEXT((#1587))
GLOBAL_UNIT_ASSIGNED_CONTEXT((#1603,#1605,#1606))
REPRESENTATION_CONTEXT('','3D')
);
#1598=(
GEOMETRIC_REPRESENTATION_CONTEXT(3)
GLOBAL_UNCERTAINTY_ASSIGNED_CONTEXT((#1588))
GLOBAL_UNIT_ASSIGNED_CONTEXT((#1603,#1605,#1606))
REPRESENTATION_CONTEXT('','3D')
);
#1599=(
GEOMETRIC_REPRESENTATION_CONTEXT(3)
GLOBAL_UNCERTAINTY_ASSIGNED_CONTEXT((#1589))
GLOBAL_UNIT_ASSIGNED_CONTEXT((#1603,#1605,#1606))
REPRESENTATION_CONTEXT('','3D')
);
#1600=(
GEOMETRIC_REPRESENTATION_CONTEXT(3)
GLOBAL_UNCERTAINTY_ASSIGNED_CONTEXT((#1590))
GLOBAL_UNIT_ASSIGNED_CONTEXT((#1603,#1605,#1606))
REPRESENTATION_CONTEXT('','3D')
);
#1601=(
GEOMETRIC_REPRESENTATION_CONTEXT(3)
GLOBAL_UNCERTAINTY_ASSIGNED_CONTEXT((#1591))
GLOBAL_UNIT_ASSIGNED_CONTEXT((#1603,#1605,#1606))
REPRESENTATION_CONTEXT('','3D')
);
#1602=(
GEOMETRIC_REPRESENTATION_CONTEXT(3)
GLOBAL_UNCERTAINTY_ASSIGNED_CONTEXT((#1592))
GLOBAL_UNIT_ASSIGNED_CONTEXT((#1603,#1605,#1606))
REPRESENTATION_CONTEXT('','3D')
);
#1603=(
LENGTH_UNIT()
NAMED_UNIT(*)
SI_UNIT(.MILLI.,.METRE.)
);
#1604=(
LENGTH_UNIT()
NAMED_UNIT(*)
SI_UNIT($,.METRE.)
);
#1605=(
NAMED_UNIT(*)
PLANE_ANGLE_UNIT()
SI_UNIT($,.RADIAN.)
);
#1606=(
NAMED_UNIT(*)
SI_UNIT($,.STERADIAN.)
SOLID_ANGLE_UNIT()
);
#1607=SHAPE_DEFINITION_REPRESENTATION(#1616,#1633);
#1608=SHAPE_DEFINITION_REPRESENTATION(#1617,#1634);
#1609=SHAPE_DEFINITION_REPRESENTATION(#1618,#1635);
#1610=SHAPE_DEFINITION_REPRESENTATION(#1619,#1636);
#1611=SHAPE_DEFINITION_REPRESENTATION(#1620,#1637);
#1612=SHAPE_DEFINITION_REPRESENTATION(#1621,#1638);
#1613=SHAPE_DEFINITION_REPRESENTATION(#1622,#1639);
#1614=SHAPE_DEFINITION_REPRESENTATION(#1623,#1640);
#1615=SHAPE_DEFINITION_REPRESENTATION(#1624,#1641);
#1616=PRODUCT_DEFINITION_SHAPE('',$,#1643);
#1617=PRODUCT_DEFINITION_SHAPE('',$,#1644);
#1618=PRODUCT_DEFINITION_SHAPE('',$,#1645);
#1619=PRODUCT_DEFINITION_SHAPE('',$,#1646);
#1620=PRODUCT_DEFINITION_SHAPE('',$,#1647);
#1621=PRODUCT_DEFINITION_SHAPE('',$,#1648);
#1622=PRODUCT_DEFINITION_SHAPE('',$,#1649);
#1623=PRODUCT_DEFINITION_SHAPE('',$,#1650);
#1624=PRODUCT_DEFINITION_SHAPE('',$,#1651);
#1625=PRODUCT_DEFINITION_SHAPE($,$,#35);
#1626=PRODUCT_DEFINITION_SHAPE($,$,#36);
#1627=PRODUCT_DEFINITION_SHAPE($,$,#37);
#1628=PRODUCT_DEFINITION_SHAPE($,$,#38);
#1629=PRODUCT_DEFINITION_SHAPE($,$,#39);
#1630=PRODUCT_DEFINITION_SHAPE($,$,#40);
#1631=PRODUCT_DEFINITION_SHAPE($,$,#41);
#1632=PRODUCT_DEFINITION_SHAPE($,$,#42);
#1633=SHAPE_REPRESENTATION('',(#871,#967,#968,#969,#970,#971,#972,#973,
#974),#1593);
#1634=SHAPE_REPRESENTATION('',(#872),#1594);
#1635=SHAPE_REPRESENTATION('',(#911),#1595);
#1636=SHAPE_REPRESENTATION('',(#917),#1596);
#1637=SHAPE_REPRESENTATION('',(#928),#1597);
#1638=SHAPE_REPRESENTATION('',(#934),#1598);
#1639=SHAPE_REPRESENTATION('',(#940),#1599);
#1640=SHAPE_REPRESENTATION('',(#952),#1600);
#1641=SHAPE_REPRESENTATION('',(#958),#1601);
#1642=PRODUCT_DEFINITION_CONTEXT('part definition',#1671,'design');
#1643=PRODUCT_DEFINITION('BR-053','BR-053',#1652,#1642);
#1644=PRODUCT_DEFINITION('Wheel','Wheel',#1653,#1642);
#1645=PRODUCT_DEFINITION('Pin_03','Pin_03',#1654,#1642);
#1646=PRODUCT_DEFINITION('Ring','Ring',#1655,#1642);
#1647=PRODUCT_DEFINITION('Pin_01','Pin_01',#1656,#1642);
#1648=PRODUCT_DEFINITION('Pin_02','Pin_02',#1657,#1642);
#1649=PRODUCT_DEFINITION('Crank','Crank',#1658,#1642);
#1650=PRODUCT_DEFINITION('Pin_04','Pin_04',#1659,#1642);
#1651=PRODUCT_DEFINITION('spacer','Spacer',#1660,#1642);
#1652=PRODUCT_DEFINITION_FORMATION('',$,#1673);
#1653=PRODUCT_DEFINITION_FORMATION('',$,#1674);
#1654=PRODUCT_DEFINITION_FORMATION('',$,#1675);
#1655=PRODUCT_DEFINITION_FORMATION('',$,#1676);
#1656=PRODUCT_DEFINITION_FORMATION('',$,#1677);
#1657=PRODUCT_DEFINITION_FORMATION('',$,#1678);
#1658=PRODUCT_DEFINITION_FORMATION('',$,#1679);
#1659=PRODUCT_DEFINITION_FORMATION('',$,#1680);
#1660=PRODUCT_DEFINITION_FORMATION('',$,#1681);
#1661=PRODUCT_RELATED_PRODUCT_CATEGORY('BR-053','BR-053',(#1673));
#1662=PRODUCT_RELATED_PRODUCT_CATEGORY('Wheel','Wheel',(#1674));
#1663=PRODUCT_RELATED_PRODUCT_CATEGORY('Pin_03','Pin_03',(#1675));
#1664=PRODUCT_RELATED_PRODUCT_CATEGORY('Ring','Ring',(#1676));
#1665=PRODUCT_RELATED_PRODUCT_CATEGORY('Pin_01','Pin_01',(#1677));
#1666=PRODUCT_RELATED_PRODUCT_CATEGORY('Pin_02','Pin_02',(#1678));
#1667=PRODUCT_RELATED_PRODUCT_CATEGORY('Crank','Crank',(#1679));
#1668=PRODUCT_RELATED_PRODUCT_CATEGORY('Pin_04','Pin_04',(#1680));
#1669=PRODUCT_RELATED_PRODUCT_CATEGORY('Spacer','Spacer',(#1681));
#1670=APPLICATION_PROTOCOL_DEFINITION('international standard',
'automotive_design',2009,#1671);
#1671=APPLICATION_CONTEXT(
'Core Data for Automotive Mechanical Design Process');
#1672=PRODUCT_CONTEXT('part definition',#1671,'mechanical');
#1673=PRODUCT('BR-053','BR-053',$,(#1672));
#1674=PRODUCT('Wheel','Wheel',$,(#1672));
#1675=PRODUCT('Pin_03','Pin_03',$,(#1672));
#1676=PRODUCT('Ring','Ring',$,(#1672));
#1677=PRODUCT('Pin_01','Pin_01',$,(#1672));
#1678=PRODUCT('Pin_02','Pin_02',$,(#1672));
#1679=PRODUCT('Crank','Crank',$,(#1672));
#1680=PRODUCT('Pin_04','Pin_04',$,(#1672));
#1681=PRODUCT('spacer','Spacer',$,(#1672));
#1682=PRESENTATION_STYLE_ASSIGNMENT((#1686));
#1683=PRESENTATION_STYLE_ASSIGNMENT((#1687));
#1684=PRESENTATION_STYLE_ASSIGNMENT((#1688));
#1685=PRESENTATION_STYLE_ASSIGNMENT((#1689));
#1686=SURFACE_STYLE_USAGE(.BOTH.,#1690);
#1687=SURFACE_STYLE_USAGE(.BOTH.,#1691);
#1688=SURFACE_STYLE_USAGE(.BOTH.,#1692);
#1689=SURFACE_STYLE_USAGE(.BOTH.,#1693);
#1690=SURFACE_SIDE_STYLE('',(#1694));
#1691=SURFACE_SIDE_STYLE('',(#1695));
#1692=SURFACE_SIDE_STYLE('',(#1696));
#1693=SURFACE_SIDE_STYLE('',(#1697));
#1694=SURFACE_STYLE_FILL_AREA(#1698);
#1695=SURFACE_STYLE_FILL_AREA(#1699);
#1696=SURFACE_STYLE_FILL_AREA(#1700);
#1697=SURFACE_STYLE_FILL_AREA(#1701);
#1698=FILL_AREA_STYLE('Steel - Satin',(#1702));
#1699=FILL_AREA_STYLE('Opaque(0,85,255)',(#1703));
#1700=FILL_AREA_STYLE('Opaque(160,160,160)',(#1704));
#1701=FILL_AREA_STYLE('Opaque(85,255,0)',(#1705));
#1702=FILL_AREA_STYLE_COLOUR('Steel - Satin',#1706);
#1703=FILL_AREA_STYLE_COLOUR('Opaque(0,85,255)',#1707);
#1704=FILL_AREA_STYLE_COLOUR('Opaque(160,160,160)',#1708);
#1705=FILL_AREA_STYLE_COLOUR('Opaque(85,255,0)',#1709);
#1706=COLOUR_RGB('Steel - Satin', 0.09019608, 0.27058824, 0.51372549);
#1707=COLOUR_RGB('Opaque(0,85,255)', 0.09019608, 0.27058824, 0.51372549);
#1708=COLOUR_RGB('Opaque(160,160,160)', 0.66274510, 0.83137255, 0.94901961);
#1709=COLOUR_RGB('Opaque(85,255,0)', 0.40784314, 0.44705882, 0.49803922);
ENDSEC;
END-ISO-10303-21;
